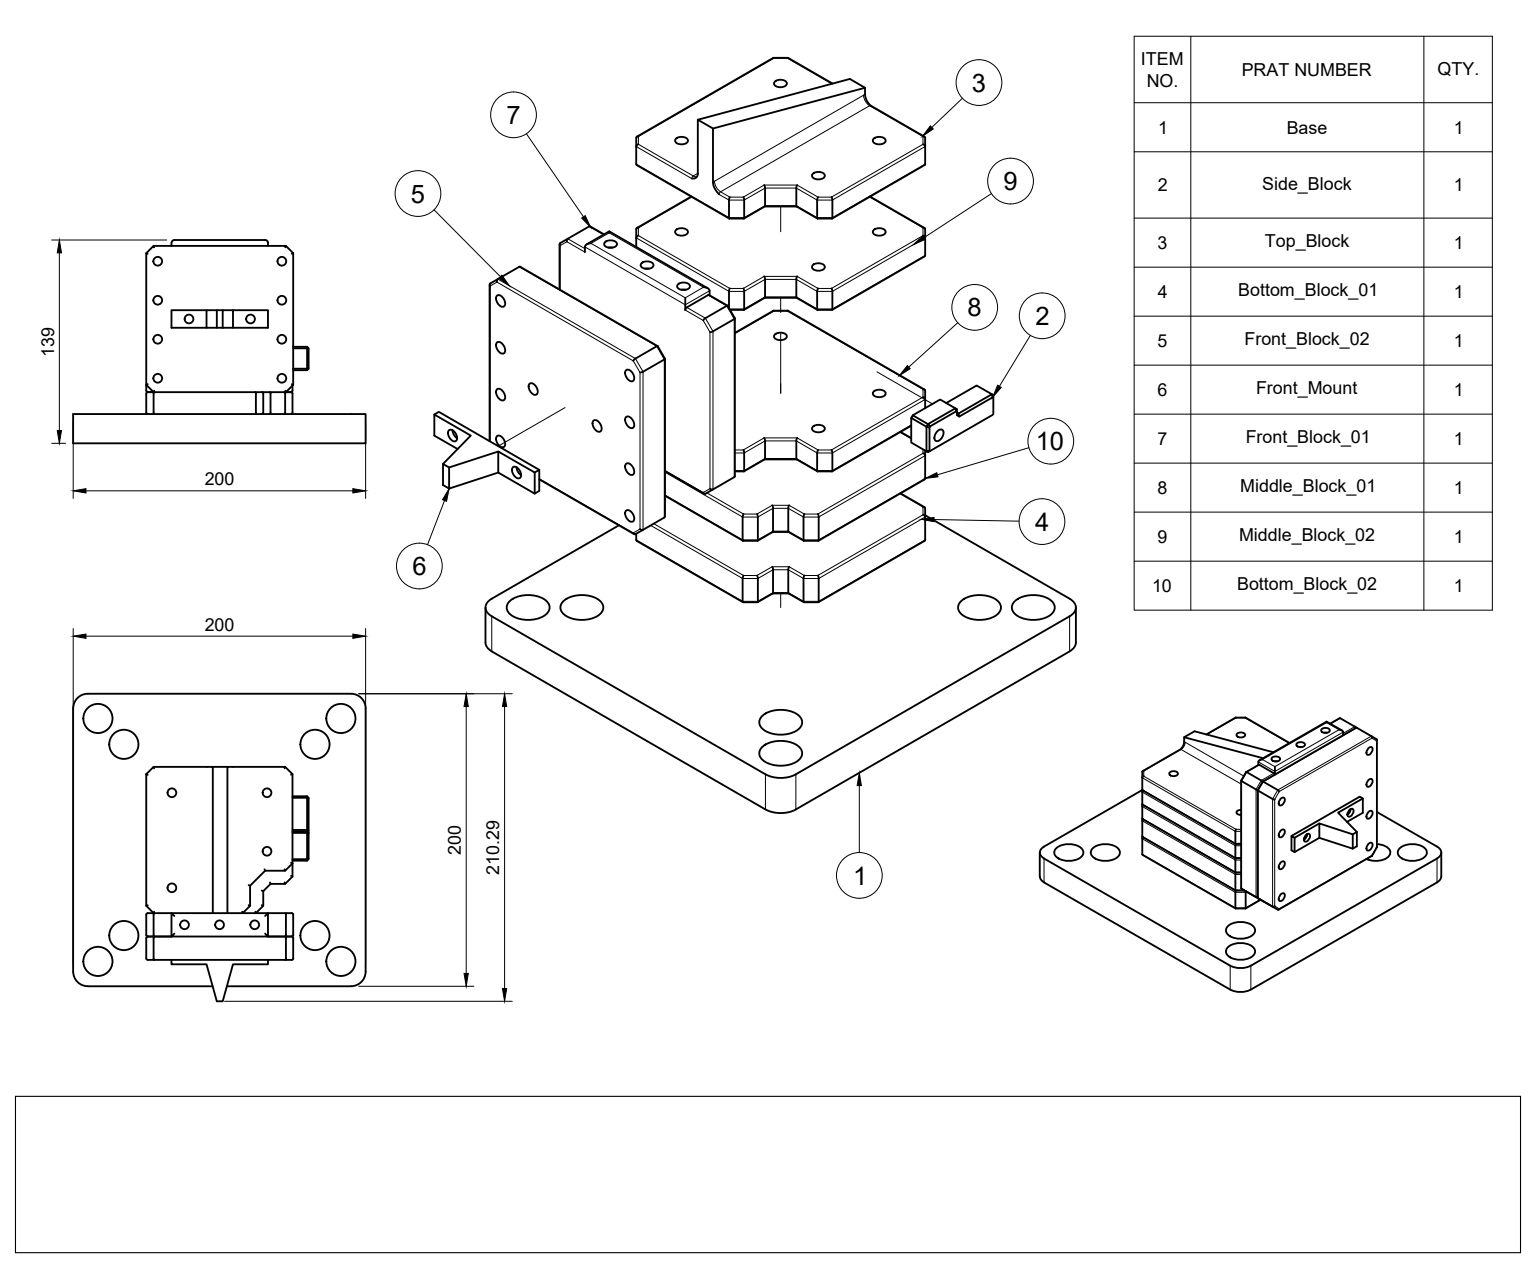
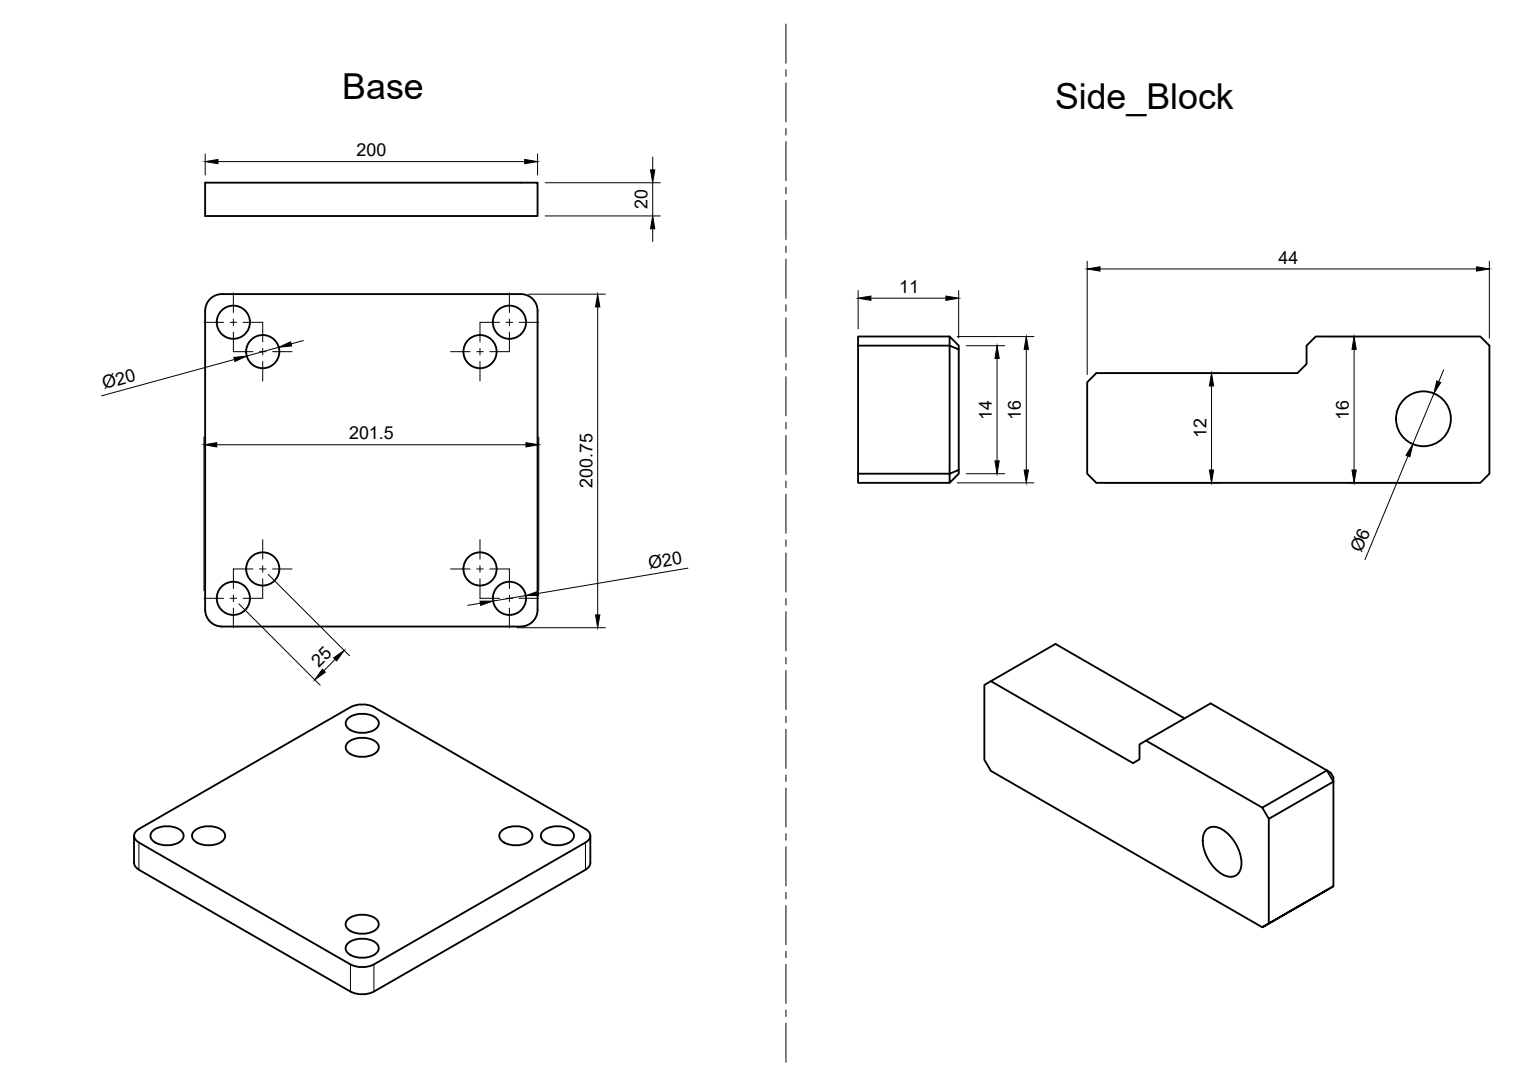
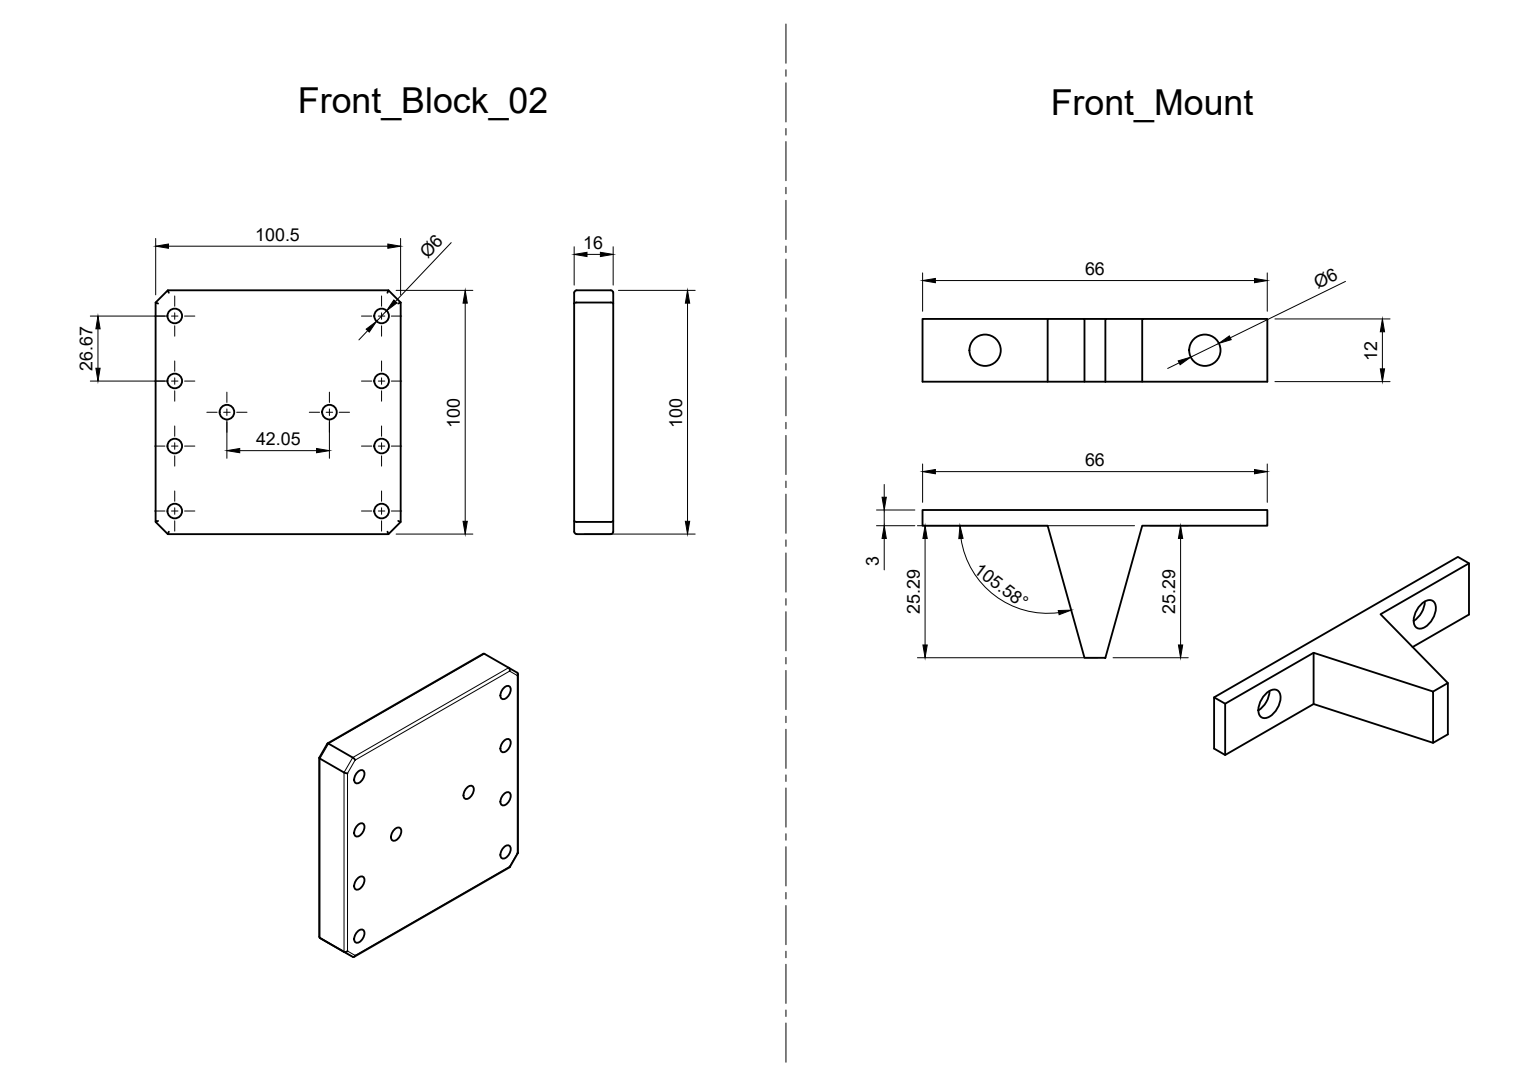
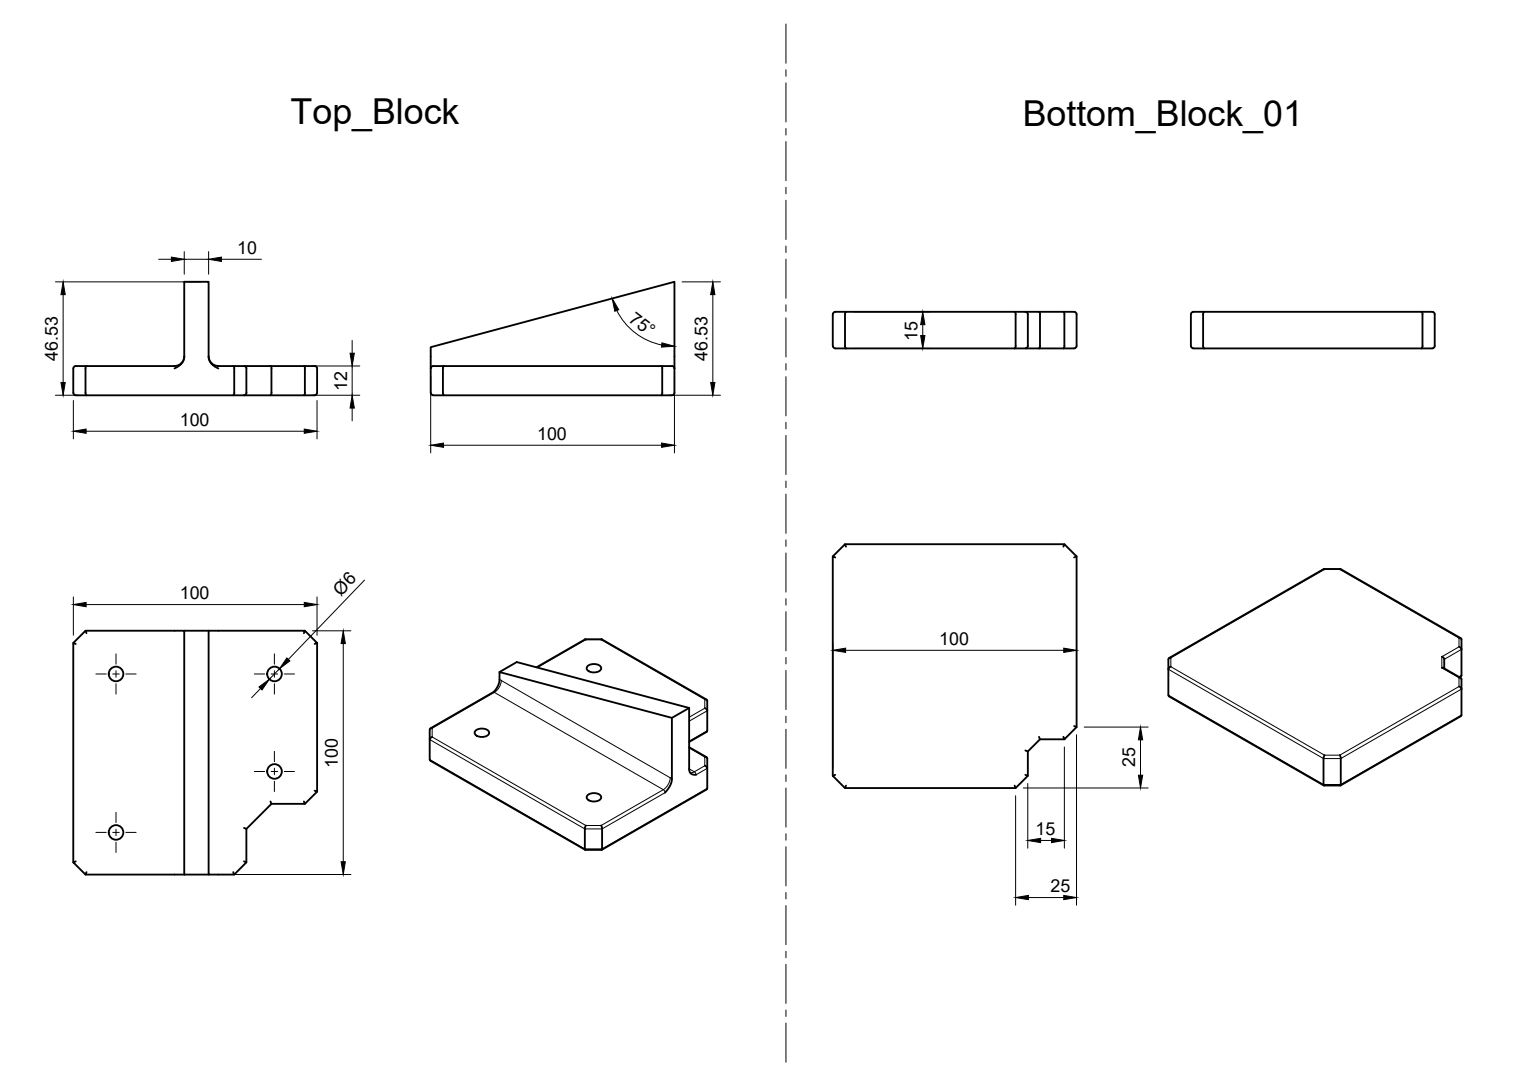
ISO-10303-21;
HEADER;
/* Generated by software containing ST-Developer
 * from STEP Tools, Inc. (www.steptools.com) 
 */

FILE_DESCRIPTION(
/* description */ (''),
/* implementation_level */ '2;1');

FILE_NAME(
/* name */ 'MAS-266',
/* time_stamp */ '2026-10-23T22:30:33+06:00',
/* author */ (''),
/* organization */ (''),
/* preprocessor_version */ 'ST-DEVELOPER v20.2',
/* originating_system */ 'Autodesk Translation Framework v15.15.0.0',
/* authorisation */ '');

FILE_SCHEMA (('AUTOMOTIVE_DESIGN { 1 0 10303 214 3 1 1 }'));
ENDSEC;

DATA;
#10=MECHANICAL_DESIGN_GEOMETRIC_PRESENTATION_REPRESENTATION('',(#235,#236,
#237,#238,#239,#240,#241,#242,#243,#244),#10131);
#11=ITEM_DEFINED_TRANSFORMATION($,$,#6001,#6612);
#12=ITEM_DEFINED_TRANSFORMATION($,$,#6044,#6613);
#13=ITEM_DEFINED_TRANSFORMATION($,$,#6074,#6614);
#14=ITEM_DEFINED_TRANSFORMATION($,$,#6173,#6615);
#15=ITEM_DEFINED_TRANSFORMATION($,$,#6236,#6616);
#16=ITEM_DEFINED_TRANSFORMATION($,$,#6309,#6617);
#17=ITEM_DEFINED_TRANSFORMATION($,$,#6326,#6618);
#18=ITEM_DEFINED_TRANSFORMATION($,$,#6399,#6619);
#19=ITEM_DEFINED_TRANSFORMATION($,$,#6474,#6620);
#20=ITEM_DEFINED_TRANSFORMATION($,$,#6549,#6621);
#21=(
REPRESENTATION_RELATIONSHIP($,$,#10169,#10168)
REPRESENTATION_RELATIONSHIP_WITH_TRANSFORMATION(#11)
SHAPE_REPRESENTATION_RELATIONSHIP()
);
#22=(
REPRESENTATION_RELATIONSHIP($,$,#10170,#10168)
REPRESENTATION_RELATIONSHIP_WITH_TRANSFORMATION(#12)
SHAPE_REPRESENTATION_RELATIONSHIP()
);
#23=(
REPRESENTATION_RELATIONSHIP($,$,#10171,#10168)
REPRESENTATION_RELATIONSHIP_WITH_TRANSFORMATION(#13)
SHAPE_REPRESENTATION_RELATIONSHIP()
);
#24=(
REPRESENTATION_RELATIONSHIP($,$,#10172,#10168)
REPRESENTATION_RELATIONSHIP_WITH_TRANSFORMATION(#14)
SHAPE_REPRESENTATION_RELATIONSHIP()
);
#25=(
REPRESENTATION_RELATIONSHIP($,$,#10173,#10168)
REPRESENTATION_RELATIONSHIP_WITH_TRANSFORMATION(#15)
SHAPE_REPRESENTATION_RELATIONSHIP()
);
#26=(
REPRESENTATION_RELATIONSHIP($,$,#10174,#10168)
REPRESENTATION_RELATIONSHIP_WITH_TRANSFORMATION(#16)
SHAPE_REPRESENTATION_RELATIONSHIP()
);
#27=(
REPRESENTATION_RELATIONSHIP($,$,#10175,#10168)
REPRESENTATION_RELATIONSHIP_WITH_TRANSFORMATION(#17)
SHAPE_REPRESENTATION_RELATIONSHIP()
);
#28=(
REPRESENTATION_RELATIONSHIP($,$,#10176,#10168)
REPRESENTATION_RELATIONSHIP_WITH_TRANSFORMATION(#18)
SHAPE_REPRESENTATION_RELATIONSHIP()
);
#29=(
REPRESENTATION_RELATIONSHIP($,$,#10177,#10168)
REPRESENTATION_RELATIONSHIP_WITH_TRANSFORMATION(#19)
SHAPE_REPRESENTATION_RELATIONSHIP()
);
#30=(
REPRESENTATION_RELATIONSHIP($,$,#10178,#10168)
REPRESENTATION_RELATIONSHIP_WITH_TRANSFORMATION(#20)
SHAPE_REPRESENTATION_RELATIONSHIP()
);
#31=CONTEXT_DEPENDENT_SHAPE_REPRESENTATION(#21,#10158);
#32=CONTEXT_DEPENDENT_SHAPE_REPRESENTATION(#22,#10159);
#33=CONTEXT_DEPENDENT_SHAPE_REPRESENTATION(#23,#10160);
#34=CONTEXT_DEPENDENT_SHAPE_REPRESENTATION(#24,#10161);
#35=CONTEXT_DEPENDENT_SHAPE_REPRESENTATION(#25,#10162);
#36=CONTEXT_DEPENDENT_SHAPE_REPRESENTATION(#26,#10163);
#37=CONTEXT_DEPENDENT_SHAPE_REPRESENTATION(#27,#10164);
#38=CONTEXT_DEPENDENT_SHAPE_REPRESENTATION(#28,#10165);
#39=CONTEXT_DEPENDENT_SHAPE_REPRESENTATION(#29,#10166);
#40=CONTEXT_DEPENDENT_SHAPE_REPRESENTATION(#30,#10167);
#41=NEXT_ASSEMBLY_USAGE_OCCURRENCE('Base:1','Base:1','Base:1',#10180,#10181,
'Base:1');
#42=NEXT_ASSEMBLY_USAGE_OCCURRENCE('Side_Block:1','Side_Block:1',
'Side_Block:1',#10180,#10182,'Side_Block:1');
#43=NEXT_ASSEMBLY_USAGE_OCCURRENCE('Top_Block:1','Top_Block:1',
'Top_Block:1',#10180,#10183,'Top_Block:1');
#44=NEXT_ASSEMBLY_USAGE_OCCURRENCE('Bottom_Block_01:1',
'Bottom_Block_01:1','Bottom_Block_01:1',#10180,#10184,
'Bottom_Block_01:1');
#45=NEXT_ASSEMBLY_USAGE_OCCURRENCE('Front_Block_02:1',
'Front_Block_02:1','Front_Block_02:1',#10180,#10185,'Front_Block_02:1');
#46=NEXT_ASSEMBLY_USAGE_OCCURRENCE('Front_Mount:1','Front_Mount:1',
'Front_Mount:1',#10180,#10186,'Front_Mount:1');
#47=NEXT_ASSEMBLY_USAGE_OCCURRENCE('Front_Block_01:1',
'Front_Block_01:1','Front_Block_01:1',#10180,#10187,'Front_Block_01:1');
#48=NEXT_ASSEMBLY_USAGE_OCCURRENCE('Middle_Block_01:1',
'Middle_Block_01:1','Middle_Block_01:1',#10180,#10188,
'Middle_Block_01:1');
#49=NEXT_ASSEMBLY_USAGE_OCCURRENCE('Middle_Block_02:1',
'Middle_Block_02:1','Middle_Block_02:1',#10180,#10189,
'Middle_Block_02:1');
#50=NEXT_ASSEMBLY_USAGE_OCCURRENCE('Bottom_Block_02:1',
'Bottom_Block_02:1','Bottom_Block_02:1',#10180,#10190,
'Bottom_Block_02:1');
#51=ELLIPSE('',#6109,1.08239220029239,1.);
#52=ELLIPSE('',#6111,1.08239220029239,1.);
#53=ELLIPSE('',#6115,1.08239220029239,1.);
#54=ELLIPSE('',#6117,1.08239220029239,1.);
#55=ELLIPSE('',#6119,1.0823922002924,1.);
#56=ELLIPSE('',#6120,1.08239220029239,1.);
#57=ELLIPSE('',#6122,1.08239220029239,1.);
#58=ELLIPSE('',#6123,1.0823922002924,1.);
#59=ELLIPSE('',#6125,1.0823922002924,1.);
#60=ELLIPSE('',#6127,1.0823922002924,1.);
#61=ELLIPSE('',#6128,1.0823922002924,1.);
#62=ELLIPSE('',#6130,1.08239220029239,1.);
#63=ELLIPSE('',#6133,1.08239220029239,1.);
#64=ELLIPSE('',#6135,1.0823922002924,1.);
#65=ELLIPSE('',#6138,1.08239220029239,1.);
#66=ELLIPSE('',#6140,1.0823922002924,1.);
#67=ELLIPSE('',#6150,1.08239220029239,1.);
#68=ELLIPSE('',#6152,1.08239220029239,1.);
#69=ELLIPSE('',#6155,1.08239220029239,1.);
#70=ELLIPSE('',#6157,1.0823922002924,1.);
#71=ELLIPSE('',#6159,1.08239220029239,1.);
#72=ELLIPSE('',#6161,1.08239220029239,1.);
#73=ELLIPSE('',#6163,1.0823922002924,1.);
#74=ELLIPSE('',#6165,1.0823922002924,1.);
#75=ELLIPSE('',#6175,1.08239220029239,1.);
#76=ELLIPSE('',#6176,1.08239220029239,1.);
#77=ELLIPSE('',#6178,1.08239220029239,1.);
#78=ELLIPSE('',#6179,1.08239220029239,1.);
#79=ELLIPSE('',#6181,1.08239220029239,1.);
#80=ELLIPSE('',#6183,1.0823922002924,1.);
#81=ELLIPSE('',#6185,1.08239220029239,1.);
#82=ELLIPSE('',#6187,1.0823922002924,1.);
#83=ELLIPSE('',#6189,1.08239220029239,1.);
#84=ELLIPSE('',#6191,1.0823922002924,1.);
#85=ELLIPSE('',#6193,1.08239220029239,1.);
#86=ELLIPSE('',#6195,1.0823922002924,1.);
#87=ELLIPSE('',#6206,1.08239220029239,1.);
#88=ELLIPSE('',#6207,1.0823922002924,1.);
#89=ELLIPSE('',#6209,1.08239220029239,1.);
#90=ELLIPSE('',#6211,1.0823922002924,1.);
#91=ELLIPSE('',#6213,1.08239220029239,1.);
#92=ELLIPSE('',#6215,1.0823922002924,1.);
#93=ELLIPSE('',#6217,1.08239220029239,1.);
#94=ELLIPSE('',#6219,1.0823922002924,1.);
#95=ELLIPSE('',#6221,1.08239220029239,1.);
#96=ELLIPSE('',#6223,1.0823922002924,1.);
#97=ELLIPSE('',#6225,1.08239220029239,1.);
#98=ELLIPSE('',#6227,1.08239220029239,1.);
#99=ELLIPSE('',#6268,1.0823922002924,1.);
#100=ELLIPSE('',#6269,1.0823922002924,1.);
#101=ELLIPSE('',#6271,1.08239220029239,1.);
#102=ELLIPSE('',#6273,1.0823922002924,1.);
#103=ELLIPSE('',#6275,1.08239220029239,1.);
#104=ELLIPSE('',#6277,1.0823922002924,1.);
#105=ELLIPSE('',#6279,1.0823922002924,1.);
#106=ELLIPSE('',#6281,1.08239220029239,1.);
#107=ELLIPSE('',#6289,1.0823922002924,1.);
#108=ELLIPSE('',#6290,1.08239220029239,1.);
#109=ELLIPSE('',#6292,1.08239220029239,1.);
#110=ELLIPSE('',#6294,1.08239220029239,1.);
#111=ELLIPSE('',#6296,1.08239220029239,1.);
#112=ELLIPSE('',#6298,1.0823922002924,1.);
#113=ELLIPSE('',#6300,1.08239220029239,1.);
#114=ELLIPSE('',#6302,1.0823922002924,1.);
#115=ELLIPSE('',#6340,2.82842712474619,2.);
#116=ELLIPSE('',#6341,2.82842712474619,2.);
#117=ELLIPSE('',#6343,2.8284271247462,2.);
#118=ELLIPSE('',#6345,2.8284271247462,2.);
#119=ELLIPSE('',#6357,1.08239220029239,1.);
#120=ELLIPSE('',#6359,1.0823922002924,1.);
#121=ELLIPSE('',#6362,1.0823922002924,1.);
#122=ELLIPSE('',#6364,1.0823922002924,1.);
#123=ELLIPSE('',#6365,1.0823922002924,1.);
#124=ELLIPSE('',#6367,1.08239220029239,1.);
#125=ELLIPSE('',#6369,1.0823922002924,1.);
#126=ELLIPSE('',#6371,1.08239220029239,1.);
#127=ELLIPSE('',#6373,1.0823922002924,1.);
#128=ELLIPSE('',#6381,1.0823922002924,1.);
#129=ELLIPSE('',#6382,1.08239220029239,1.);
#130=ELLIPSE('',#6384,1.08239220029239,1.);
#131=ELLIPSE('',#6386,1.08239220029239,1.);
#132=ELLIPSE('',#6388,1.08239220029239,1.);
#133=ELLIPSE('',#6390,1.0823922002924,1.);
#134=ELLIPSE('',#6392,1.08239220029239,1.);
#135=ELLIPSE('',#6413,1.0823922002924,1.);
#136=ELLIPSE('',#6414,1.08239220029239,1.);
#137=ELLIPSE('',#6416,1.08239220029239,1.);
#138=ELLIPSE('',#6417,1.0823922002924,1.);
#139=ELLIPSE('',#6419,1.0823922002924,1.);
#140=ELLIPSE('',#6421,1.0823922002924,1.);
#141=ELLIPSE('',#6422,1.0823922002924,1.);
#142=ELLIPSE('',#6424,1.08239220029239,1.);
#143=ELLIPSE('',#6427,1.08239220029239,1.);
#144=ELLIPSE('',#6429,1.0823922002924,1.);
#145=ELLIPSE('',#6432,1.08239220029239,1.);
#146=ELLIPSE('',#6434,1.0823922002924,1.);
#147=ELLIPSE('',#6444,1.08239220029239,1.);
#148=ELLIPSE('',#6445,1.08239220029239,1.);
#149=ELLIPSE('',#6447,1.08239220029239,1.);
#150=ELLIPSE('',#6449,1.08239220029239,1.);
#151=ELLIPSE('',#6451,1.08239220029239,1.);
#152=ELLIPSE('',#6453,1.08239220029239,1.);
#153=ELLIPSE('',#6455,1.0823922002924,1.);
#154=ELLIPSE('',#6457,1.08239220029239,1.);
#155=ELLIPSE('',#6459,1.08239220029239,1.);
#156=ELLIPSE('',#6461,1.0823922002924,1.);
#157=ELLIPSE('',#6463,1.0823922002924,1.);
#158=ELLIPSE('',#6465,1.08239220029239,1.);
#159=ELLIPSE('',#6488,1.0823922002924,1.);
#160=ELLIPSE('',#6489,1.08239220029239,1.);
#161=ELLIPSE('',#6491,1.08239220029239,1.);
#162=ELLIPSE('',#6492,1.0823922002924,1.);
#163=ELLIPSE('',#6494,1.0823922002924,1.);
#164=ELLIPSE('',#6496,1.0823922002924,1.);
#165=ELLIPSE('',#6497,1.0823922002924,1.);
#166=ELLIPSE('',#6499,1.08239220029239,1.);
#167=ELLIPSE('',#6502,1.08239220029239,1.);
#168=ELLIPSE('',#6504,1.0823922002924,1.);
#169=ELLIPSE('',#6507,1.08239220029239,1.);
#170=ELLIPSE('',#6509,1.0823922002924,1.);
#171=ELLIPSE('',#6519,1.08239220029239,1.);
#172=ELLIPSE('',#6520,1.08239220029239,1.);
#173=ELLIPSE('',#6522,1.08239220029239,1.);
#174=ELLIPSE('',#6524,1.08239220029239,1.);
#175=ELLIPSE('',#6526,1.08239220029239,1.);
#176=ELLIPSE('',#6528,1.08239220029239,1.);
#177=ELLIPSE('',#6530,1.0823922002924,1.);
#178=ELLIPSE('',#6532,1.08239220029239,1.);
#179=ELLIPSE('',#6534,1.08239220029239,1.);
#180=ELLIPSE('',#6536,1.0823922002924,1.);
#181=ELLIPSE('',#6538,1.0823922002924,1.);
#182=ELLIPSE('',#6540,1.08239220029239,1.);
#183=ELLIPSE('',#6551,1.08239220029239,1.);
#184=ELLIPSE('',#6552,1.08239220029239,1.);
#185=ELLIPSE('',#6554,1.08239220029239,1.);
#186=ELLIPSE('',#6555,1.08239220029239,1.);
#187=ELLIPSE('',#6557,1.08239220029239,1.);
#188=ELLIPSE('',#6559,1.0823922002924,1.);
#189=ELLIPSE('',#6561,1.08239220029239,1.);
#190=ELLIPSE('',#6563,1.0823922002924,1.);
#191=ELLIPSE('',#6565,1.08239220029239,1.);
#192=ELLIPSE('',#6567,1.0823922002924,1.);
#193=ELLIPSE('',#6569,1.08239220029239,1.);
#194=ELLIPSE('',#6571,1.0823922002924,1.);
#195=ELLIPSE('',#6582,1.08239220029239,1.);
#196=ELLIPSE('',#6583,1.0823922002924,1.);
#197=ELLIPSE('',#6585,1.08239220029239,1.);
#198=ELLIPSE('',#6587,1.0823922002924,1.);
#199=ELLIPSE('',#6589,1.08239220029239,1.);
#200=ELLIPSE('',#6591,1.0823922002924,1.);
#201=ELLIPSE('',#6593,1.08239220029239,1.);
#202=ELLIPSE('',#6595,1.0823922002924,1.);
#203=ELLIPSE('',#6597,1.08239220029239,1.);
#204=ELLIPSE('',#6599,1.0823922002924,1.);
#205=ELLIPSE('',#6601,1.08239220029239,1.);
#206=ELLIPSE('',#6603,1.08239220029239,1.);
#207=B_SPLINE_CURVE_WITH_KNOTS('',3,(#8653,#8654,#8655,#8656,#8657,#8658,
#8659,#8660,#8661,#8662),.UNSPECIFIED.,.F.,.F.,(4,2,2,2,4),(0.,0.179989683878213,
0.359979367756426,0.499959890996325,0.633875417351683),.UNSPECIFIED.);
#208=B_SPLINE_CURVE_WITH_KNOTS('',3,(#8673,#8674,#8675,#8676,#8677,#8678,
#8679,#8680,#8681,#8682),.UNSPECIFIED.,.F.,.F.,(4,2,2,2,4),(1.82590429893059,
1.95981982528595,2.09980034852585,2.27979003240406,2.45977971628227),
 .UNSPECIFIED.);
#209=B_SPLINE_CURVE_WITH_KNOTS('',3,(#8698,#8699,#8700,#8701,#8702,#8703,
#8704,#8705,#8706,#8707),.UNSPECIFIED.,.F.,.F.,(4,2,2,2,4),(0.,0.179989683878213,
0.359979367756426,0.499959890996325,0.633875417351683),.UNSPECIFIED.);
#210=B_SPLINE_CURVE_WITH_KNOTS('',3,(#8718,#8719,#8720,#8721,#8722,#8723,
#8724,#8725,#8726,#8727),.UNSPECIFIED.,.F.,.F.,(4,2,2,2,4),(1.82590429893059,
1.95981982528595,2.09980034852585,2.27979003240406,2.45977971628227),
 .UNSPECIFIED.);
#211=TOROIDAL_SURFACE('',#6075,5.,4.);
#212=TOROIDAL_SURFACE('',#6081,5.,4.);
#213=TOROIDAL_SURFACE('',#6085,5.,4.);
#214=TOROIDAL_SURFACE('',#6091,5.,4.);
#215=SHAPE_REPRESENTATION_RELATIONSHIP('SRR','None',#10169,#225);
#216=SHAPE_REPRESENTATION_RELATIONSHIP('SRR','None',#10170,#226);
#217=SHAPE_REPRESENTATION_RELATIONSHIP('SRR','None',#10171,#227);
#218=SHAPE_REPRESENTATION_RELATIONSHIP('SRR','None',#10172,#228);
#219=SHAPE_REPRESENTATION_RELATIONSHIP('SRR','None',#10173,#229);
#220=SHAPE_REPRESENTATION_RELATIONSHIP('SRR','None',#10174,#230);
#221=SHAPE_REPRESENTATION_RELATIONSHIP('SRR','None',#10175,#231);
#222=SHAPE_REPRESENTATION_RELATIONSHIP('SRR','None',#10176,#232);
#223=SHAPE_REPRESENTATION_RELATIONSHIP('SRR','None',#10177,#233);
#224=SHAPE_REPRESENTATION_RELATIONSHIP('SRR','None',#10178,#234);
#225=ADVANCED_BREP_SHAPE_REPRESENTATION('',(#245),#10121);
#226=ADVANCED_BREP_SHAPE_REPRESENTATION('',(#246),#10122);
#227=ADVANCED_BREP_SHAPE_REPRESENTATION('',(#247),#10123);
#228=ADVANCED_BREP_SHAPE_REPRESENTATION('',(#248),#10124);
#229=ADVANCED_BREP_SHAPE_REPRESENTATION('',(#249),#10125);
#230=ADVANCED_BREP_SHAPE_REPRESENTATION('',(#250),#10126);
#231=ADVANCED_BREP_SHAPE_REPRESENTATION('',(#251),#10127);
#232=ADVANCED_BREP_SHAPE_REPRESENTATION('',(#252),#10128);
#233=ADVANCED_BREP_SHAPE_REPRESENTATION('',(#253),#10129);
#234=ADVANCED_BREP_SHAPE_REPRESENTATION('',(#254),#10130);
#235=STYLED_ITEM('',(#10247),#245);
#236=STYLED_ITEM('',(#10247),#246);
#237=STYLED_ITEM('',(#10247),#247);
#238=STYLED_ITEM('',(#10247),#248);
#239=STYLED_ITEM('',(#10247),#249);
#240=STYLED_ITEM('',(#10261),#250);
#241=STYLED_ITEM('',(#10247),#251);
#242=STYLED_ITEM('',(#10247),#252);
#243=STYLED_ITEM('',(#10247),#253);
#244=STYLED_ITEM('',(#10247),#254);
#245=MANIFOLD_SOLID_BREP('Base',#5879);
#246=MANIFOLD_SOLID_BREP('Side_Block',#5880);
#247=MANIFOLD_SOLID_BREP('Top_Block',#5881);
#248=MANIFOLD_SOLID_BREP('Bottom_Block_01',#5882);
#249=MANIFOLD_SOLID_BREP('Front_Block_02',#5883);
#250=MANIFOLD_SOLID_BREP('Front_Mount',#5884);
#251=MANIFOLD_SOLID_BREP('Front_Block_01',#5885);
#252=MANIFOLD_SOLID_BREP('Middle_Block_01',#5886);
#253=MANIFOLD_SOLID_BREP('Middle_Block_02',#5887);
#254=MANIFOLD_SOLID_BREP('Bottom_Block_02',#5888);
#255=FACE_BOUND('',#827,.T.);
#256=FACE_BOUND('',#828,.T.);
#257=FACE_BOUND('',#829,.T.);
#258=FACE_BOUND('',#830,.T.);
#259=FACE_BOUND('',#831,.T.);
#260=FACE_BOUND('',#832,.T.);
#261=FACE_BOUND('',#833,.T.);
#262=FACE_BOUND('',#834,.T.);
#263=FACE_BOUND('',#842,.T.);
#264=FACE_BOUND('',#843,.T.);
#265=FACE_BOUND('',#844,.T.);
#266=FACE_BOUND('',#845,.T.);
#267=FACE_BOUND('',#846,.T.);
#268=FACE_BOUND('',#847,.T.);
#269=FACE_BOUND('',#848,.T.);
#270=FACE_BOUND('',#849,.T.);
#271=FACE_BOUND('',#870,.T.);
#272=FACE_BOUND('',#874,.T.);
#273=FACE_BOUND('',#895,.T.);
#274=FACE_BOUND('',#896,.T.);
#275=FACE_BOUND('',#898,.T.);
#276=FACE_BOUND('',#899,.T.);
#277=FACE_BOUND('',#921,.T.);
#278=FACE_BOUND('',#922,.T.);
#279=FACE_BOUND('',#923,.T.);
#280=FACE_BOUND('',#924,.T.);
#281=FACE_BOUND('',#1002,.T.);
#282=FACE_BOUND('',#1003,.T.);
#283=FACE_BOUND('',#1004,.T.);
#284=FACE_BOUND('',#1005,.T.);
#285=FACE_BOUND('',#1006,.T.);
#286=FACE_BOUND('',#1007,.T.);
#287=FACE_BOUND('',#1008,.T.);
#288=FACE_BOUND('',#1009,.T.);
#289=FACE_BOUND('',#1010,.T.);
#290=FACE_BOUND('',#1011,.T.);
#291=FACE_BOUND('',#1024,.T.);
#292=FACE_BOUND('',#1025,.T.);
#293=FACE_BOUND('',#1026,.T.);
#294=FACE_BOUND('',#1027,.T.);
#295=FACE_BOUND('',#1028,.T.);
#296=FACE_BOUND('',#1029,.T.);
#297=FACE_BOUND('',#1030,.T.);
#298=FACE_BOUND('',#1031,.T.);
#299=FACE_BOUND('',#1032,.T.);
#300=FACE_BOUND('',#1033,.T.);
#301=FACE_BOUND('',#1040,.T.);
#302=FACE_BOUND('',#1043,.T.);
#303=FACE_BOUND('',#1044,.T.);
#304=FACE_BOUND('',#1047,.T.);
#305=FACE_BOUND('',#1064,.T.);
#306=FACE_BOUND('',#1065,.T.);
#307=FACE_BOUND('',#1066,.T.);
#308=FACE_BOUND('',#1119,.T.);
#309=FACE_BOUND('',#1120,.T.);
#310=FACE_BOUND('',#1121,.T.);
#311=FACE_BOUND('',#1122,.T.);
#312=FACE_BOUND('',#1138,.T.);
#313=FACE_BOUND('',#1139,.T.);
#314=FACE_BOUND('',#1140,.T.);
#315=FACE_BOUND('',#1141,.T.);
#316=FACE_BOUND('',#1169,.T.);
#317=FACE_BOUND('',#1170,.T.);
#318=FACE_BOUND('',#1171,.T.);
#319=FACE_BOUND('',#1172,.T.);
#320=FACE_BOUND('',#1188,.T.);
#321=FACE_BOUND('',#1189,.T.);
#322=FACE_BOUND('',#1190,.T.);
#323=FACE_BOUND('',#1191,.T.);
#324=PLANE('',#6029);
#325=PLANE('',#6030);
#326=PLANE('',#6036);
#327=PLANE('',#6041);
#328=PLANE('',#6042);
#329=PLANE('',#6043);
#330=PLANE('',#6048);
#331=PLANE('',#6049);
#332=PLANE('',#6050);
#333=PLANE('',#6051);
#334=PLANE('',#6052);
#335=PLANE('',#6053);
#336=PLANE('',#6054);
#337=PLANE('',#6055);
#338=PLANE('',#6056);
#339=PLANE('',#6057);
#340=PLANE('',#6058);
#341=PLANE('',#6059);
#342=PLANE('',#6060);
#343=PLANE('',#6061);
#344=PLANE('',#6062);
#345=PLANE('',#6063);
#346=PLANE('',#6064);
#347=PLANE('',#6065);
#348=PLANE('',#6066);
#349=PLANE('',#6067);
#350=PLANE('',#6068);
#351=PLANE('',#6069);
#352=PLANE('',#6070);
#353=PLANE('',#6071);
#354=PLANE('',#6072);
#355=PLANE('',#6073);
#356=PLANE('',#6084);
#357=PLANE('',#6094);
#358=PLANE('',#6107);
#359=PLANE('',#6112);
#360=PLANE('',#6113);
#361=PLANE('',#6142);
#362=PLANE('',#6143);
#363=PLANE('',#6144);
#364=PLANE('',#6145);
#365=PLANE('',#6146);
#366=PLANE('',#6147);
#367=PLANE('',#6148);
#368=PLANE('',#6167);
#369=PLANE('',#6168);
#370=PLANE('',#6169);
#371=PLANE('',#6170);
#372=PLANE('',#6171);
#373=PLANE('',#6172);
#374=PLANE('',#6198);
#375=PLANE('',#6199);
#376=PLANE('',#6200);
#377=PLANE('',#6201);
#378=PLANE('',#6202);
#379=PLANE('',#6203);
#380=PLANE('',#6204);
#381=PLANE('',#6229);
#382=PLANE('',#6230);
#383=PLANE('',#6231);
#384=PLANE('',#6232);
#385=PLANE('',#6233);
#386=PLANE('',#6234);
#387=PLANE('',#6235);
#388=PLANE('',#6283);
#389=PLANE('',#6284);
#390=PLANE('',#6285);
#391=PLANE('',#6286);
#392=PLANE('',#6287);
#393=PLANE('',#6304);
#394=PLANE('',#6305);
#395=PLANE('',#6306);
#396=PLANE('',#6307);
#397=PLANE('',#6308);
#398=PLANE('',#6316);
#399=PLANE('',#6317);
#400=PLANE('',#6318);
#401=PLANE('',#6319);
#402=PLANE('',#6320);
#403=PLANE('',#6321);
#404=PLANE('',#6322);
#405=PLANE('',#6323);
#406=PLANE('',#6324);
#407=PLANE('',#6325);
#408=PLANE('',#6330);
#409=PLANE('',#6334);
#410=PLANE('',#6338);
#411=PLANE('',#6347);
#412=PLANE('',#6350);
#413=PLANE('',#6351);
#414=PLANE('',#6352);
#415=PLANE('',#6355);
#416=PLANE('',#6360);
#417=PLANE('',#6376);
#418=PLANE('',#6377);
#419=PLANE('',#6378);
#420=PLANE('',#6379);
#421=PLANE('',#6395);
#422=PLANE('',#6396);
#423=PLANE('',#6397);
#424=PLANE('',#6398);
#425=PLANE('',#6436);
#426=PLANE('',#6437);
#427=PLANE('',#6438);
#428=PLANE('',#6439);
#429=PLANE('',#6440);
#430=PLANE('',#6441);
#431=PLANE('',#6442);
#432=PLANE('',#6467);
#433=PLANE('',#6468);
#434=PLANE('',#6469);
#435=PLANE('',#6470);
#436=PLANE('',#6471);
#437=PLANE('',#6472);
#438=PLANE('',#6473);
#439=PLANE('',#6511);
#440=PLANE('',#6512);
#441=PLANE('',#6513);
#442=PLANE('',#6514);
#443=PLANE('',#6515);
#444=PLANE('',#6516);
#445=PLANE('',#6517);
#446=PLANE('',#6542);
#447=PLANE('',#6543);
#448=PLANE('',#6544);
#449=PLANE('',#6545);
#450=PLANE('',#6546);
#451=PLANE('',#6547);
#452=PLANE('',#6548);
#453=PLANE('',#6574);
#454=PLANE('',#6575);
#455=PLANE('',#6576);
#456=PLANE('',#6577);
#457=PLANE('',#6578);
#458=PLANE('',#6579);
#459=PLANE('',#6580);
#460=PLANE('',#6605);
#461=PLANE('',#6606);
#462=PLANE('',#6607);
#463=PLANE('',#6608);
#464=PLANE('',#6609);
#465=PLANE('',#6610);
#466=PLANE('',#6611);
#467=FACE_OUTER_BOUND('',#816,.T.);
#468=FACE_OUTER_BOUND('',#817,.T.);
#469=FACE_OUTER_BOUND('',#818,.T.);
#470=FACE_OUTER_BOUND('',#819,.T.);
#471=FACE_OUTER_BOUND('',#820,.T.);
#472=FACE_OUTER_BOUND('',#821,.T.);
#473=FACE_OUTER_BOUND('',#822,.T.);
#474=FACE_OUTER_BOUND('',#823,.T.);
#475=FACE_OUTER_BOUND('',#824,.T.);
#476=FACE_OUTER_BOUND('',#825,.T.);
#477=FACE_OUTER_BOUND('',#826,.T.);
#478=FACE_OUTER_BOUND('',#835,.T.);
#479=FACE_OUTER_BOUND('',#836,.T.);
#480=FACE_OUTER_BOUND('',#837,.T.);
#481=FACE_OUTER_BOUND('',#838,.T.);
#482=FACE_OUTER_BOUND('',#839,.T.);
#483=FACE_OUTER_BOUND('',#840,.T.);
#484=FACE_OUTER_BOUND('',#841,.T.);
#485=FACE_OUTER_BOUND('',#850,.T.);
#486=FACE_OUTER_BOUND('',#851,.T.);
#487=FACE_OUTER_BOUND('',#852,.T.);
#488=FACE_OUTER_BOUND('',#853,.T.);
#489=FACE_OUTER_BOUND('',#854,.T.);
#490=FACE_OUTER_BOUND('',#855,.T.);
#491=FACE_OUTER_BOUND('',#856,.T.);
#492=FACE_OUTER_BOUND('',#857,.T.);
#493=FACE_OUTER_BOUND('',#858,.T.);
#494=FACE_OUTER_BOUND('',#859,.T.);
#495=FACE_OUTER_BOUND('',#860,.T.);
#496=FACE_OUTER_BOUND('',#861,.T.);
#497=FACE_OUTER_BOUND('',#862,.T.);
#498=FACE_OUTER_BOUND('',#863,.T.);
#499=FACE_OUTER_BOUND('',#864,.T.);
#500=FACE_OUTER_BOUND('',#865,.T.);
#501=FACE_OUTER_BOUND('',#866,.T.);
#502=FACE_OUTER_BOUND('',#867,.T.);
#503=FACE_OUTER_BOUND('',#868,.T.);
#504=FACE_OUTER_BOUND('',#869,.T.);
#505=FACE_OUTER_BOUND('',#871,.T.);
#506=FACE_OUTER_BOUND('',#872,.T.);
#507=FACE_OUTER_BOUND('',#873,.T.);
#508=FACE_OUTER_BOUND('',#875,.T.);
#509=FACE_OUTER_BOUND('',#876,.T.);
#510=FACE_OUTER_BOUND('',#877,.T.);
#511=FACE_OUTER_BOUND('',#878,.T.);
#512=FACE_OUTER_BOUND('',#879,.T.);
#513=FACE_OUTER_BOUND('',#880,.T.);
#514=FACE_OUTER_BOUND('',#881,.T.);
#515=FACE_OUTER_BOUND('',#882,.T.);
#516=FACE_OUTER_BOUND('',#883,.T.);
#517=FACE_OUTER_BOUND('',#884,.T.);
#518=FACE_OUTER_BOUND('',#885,.T.);
#519=FACE_OUTER_BOUND('',#886,.T.);
#520=FACE_OUTER_BOUND('',#887,.T.);
#521=FACE_OUTER_BOUND('',#888,.T.);
#522=FACE_OUTER_BOUND('',#889,.T.);
#523=FACE_OUTER_BOUND('',#890,.T.);
#524=FACE_OUTER_BOUND('',#891,.T.);
#525=FACE_OUTER_BOUND('',#892,.T.);
#526=FACE_OUTER_BOUND('',#893,.T.);
#527=FACE_OUTER_BOUND('',#894,.T.);
#528=FACE_OUTER_BOUND('',#897,.T.);
#529=FACE_OUTER_BOUND('',#900,.T.);
#530=FACE_OUTER_BOUND('',#901,.T.);
#531=FACE_OUTER_BOUND('',#902,.T.);
#532=FACE_OUTER_BOUND('',#903,.T.);
#533=FACE_OUTER_BOUND('',#904,.T.);
#534=FACE_OUTER_BOUND('',#905,.T.);
#535=FACE_OUTER_BOUND('',#906,.T.);
#536=FACE_OUTER_BOUND('',#907,.T.);
#537=FACE_OUTER_BOUND('',#908,.T.);
#538=FACE_OUTER_BOUND('',#909,.T.);
#539=FACE_OUTER_BOUND('',#910,.T.);
#540=FACE_OUTER_BOUND('',#911,.T.);
#541=FACE_OUTER_BOUND('',#912,.T.);
#542=FACE_OUTER_BOUND('',#913,.T.);
#543=FACE_OUTER_BOUND('',#914,.T.);
#544=FACE_OUTER_BOUND('',#915,.T.);
#545=FACE_OUTER_BOUND('',#916,.T.);
#546=FACE_OUTER_BOUND('',#917,.T.);
#547=FACE_OUTER_BOUND('',#918,.T.);
#548=FACE_OUTER_BOUND('',#919,.T.);
#549=FACE_OUTER_BOUND('',#920,.T.);
#550=FACE_OUTER_BOUND('',#925,.T.);
#551=FACE_OUTER_BOUND('',#926,.T.);
#552=FACE_OUTER_BOUND('',#927,.T.);
#553=FACE_OUTER_BOUND('',#928,.T.);
#554=FACE_OUTER_BOUND('',#929,.T.);
#555=FACE_OUTER_BOUND('',#930,.T.);
#556=FACE_OUTER_BOUND('',#931,.T.);
#557=FACE_OUTER_BOUND('',#932,.T.);
#558=FACE_OUTER_BOUND('',#933,.T.);
#559=FACE_OUTER_BOUND('',#934,.T.);
#560=FACE_OUTER_BOUND('',#935,.T.);
#561=FACE_OUTER_BOUND('',#936,.T.);
#562=FACE_OUTER_BOUND('',#937,.T.);
#563=FACE_OUTER_BOUND('',#938,.T.);
#564=FACE_OUTER_BOUND('',#939,.T.);
#565=FACE_OUTER_BOUND('',#940,.T.);
#566=FACE_OUTER_BOUND('',#941,.T.);
#567=FACE_OUTER_BOUND('',#942,.T.);
#568=FACE_OUTER_BOUND('',#943,.T.);
#569=FACE_OUTER_BOUND('',#944,.T.);
#570=FACE_OUTER_BOUND('',#945,.T.);
#571=FACE_OUTER_BOUND('',#946,.T.);
#572=FACE_OUTER_BOUND('',#947,.T.);
#573=FACE_OUTER_BOUND('',#948,.T.);
#574=FACE_OUTER_BOUND('',#949,.T.);
#575=FACE_OUTER_BOUND('',#950,.T.);
#576=FACE_OUTER_BOUND('',#951,.T.);
#577=FACE_OUTER_BOUND('',#952,.T.);
#578=FACE_OUTER_BOUND('',#953,.T.);
#579=FACE_OUTER_BOUND('',#954,.T.);
#580=FACE_OUTER_BOUND('',#955,.T.);
#581=FACE_OUTER_BOUND('',#956,.T.);
#582=FACE_OUTER_BOUND('',#957,.T.);
#583=FACE_OUTER_BOUND('',#958,.T.);
#584=FACE_OUTER_BOUND('',#959,.T.);
#585=FACE_OUTER_BOUND('',#960,.T.);
#586=FACE_OUTER_BOUND('',#961,.T.);
#587=FACE_OUTER_BOUND('',#962,.T.);
#588=FACE_OUTER_BOUND('',#963,.T.);
#589=FACE_OUTER_BOUND('',#964,.T.);
#590=FACE_OUTER_BOUND('',#965,.T.);
#591=FACE_OUTER_BOUND('',#966,.T.);
#592=FACE_OUTER_BOUND('',#967,.T.);
#593=FACE_OUTER_BOUND('',#968,.T.);
#594=FACE_OUTER_BOUND('',#969,.T.);
#595=FACE_OUTER_BOUND('',#970,.T.);
#596=FACE_OUTER_BOUND('',#971,.T.);
#597=FACE_OUTER_BOUND('',#972,.T.);
#598=FACE_OUTER_BOUND('',#973,.T.);
#599=FACE_OUTER_BOUND('',#974,.T.);
#600=FACE_OUTER_BOUND('',#975,.T.);
#601=FACE_OUTER_BOUND('',#976,.T.);
#602=FACE_OUTER_BOUND('',#977,.T.);
#603=FACE_OUTER_BOUND('',#978,.T.);
#604=FACE_OUTER_BOUND('',#979,.T.);
#605=FACE_OUTER_BOUND('',#980,.T.);
#606=FACE_OUTER_BOUND('',#981,.T.);
#607=FACE_OUTER_BOUND('',#982,.T.);
#608=FACE_OUTER_BOUND('',#983,.T.);
#609=FACE_OUTER_BOUND('',#984,.T.);
#610=FACE_OUTER_BOUND('',#985,.T.);
#611=FACE_OUTER_BOUND('',#986,.T.);
#612=FACE_OUTER_BOUND('',#987,.T.);
#613=FACE_OUTER_BOUND('',#988,.T.);
#614=FACE_OUTER_BOUND('',#989,.T.);
#615=FACE_OUTER_BOUND('',#990,.T.);
#616=FACE_OUTER_BOUND('',#991,.T.);
#617=FACE_OUTER_BOUND('',#992,.T.);
#618=FACE_OUTER_BOUND('',#993,.T.);
#619=FACE_OUTER_BOUND('',#994,.T.);
#620=FACE_OUTER_BOUND('',#995,.T.);
#621=FACE_OUTER_BOUND('',#996,.T.);
#622=FACE_OUTER_BOUND('',#997,.T.);
#623=FACE_OUTER_BOUND('',#998,.T.);
#624=FACE_OUTER_BOUND('',#999,.T.);
#625=FACE_OUTER_BOUND('',#1000,.T.);
#626=FACE_OUTER_BOUND('',#1001,.T.);
#627=FACE_OUTER_BOUND('',#1012,.T.);
#628=FACE_OUTER_BOUND('',#1013,.T.);
#629=FACE_OUTER_BOUND('',#1014,.T.);
#630=FACE_OUTER_BOUND('',#1015,.T.);
#631=FACE_OUTER_BOUND('',#1016,.T.);
#632=FACE_OUTER_BOUND('',#1017,.T.);
#633=FACE_OUTER_BOUND('',#1018,.T.);
#634=FACE_OUTER_BOUND('',#1019,.T.);
#635=FACE_OUTER_BOUND('',#1020,.T.);
#636=FACE_OUTER_BOUND('',#1021,.T.);
#637=FACE_OUTER_BOUND('',#1022,.T.);
#638=FACE_OUTER_BOUND('',#1023,.T.);
#639=FACE_OUTER_BOUND('',#1034,.T.);
#640=FACE_OUTER_BOUND('',#1035,.T.);
#641=FACE_OUTER_BOUND('',#1036,.T.);
#642=FACE_OUTER_BOUND('',#1037,.T.);
#643=FACE_OUTER_BOUND('',#1038,.T.);
#644=FACE_OUTER_BOUND('',#1039,.T.);
#645=FACE_OUTER_BOUND('',#1041,.T.);
#646=FACE_OUTER_BOUND('',#1042,.T.);
#647=FACE_OUTER_BOUND('',#1045,.T.);
#648=FACE_OUTER_BOUND('',#1046,.T.);
#649=FACE_OUTER_BOUND('',#1048,.T.);
#650=FACE_OUTER_BOUND('',#1049,.T.);
#651=FACE_OUTER_BOUND('',#1050,.T.);
#652=FACE_OUTER_BOUND('',#1051,.T.);
#653=FACE_OUTER_BOUND('',#1052,.T.);
#654=FACE_OUTER_BOUND('',#1053,.T.);
#655=FACE_OUTER_BOUND('',#1054,.T.);
#656=FACE_OUTER_BOUND('',#1055,.T.);
#657=FACE_OUTER_BOUND('',#1056,.T.);
#658=FACE_OUTER_BOUND('',#1057,.T.);
#659=FACE_OUTER_BOUND('',#1058,.T.);
#660=FACE_OUTER_BOUND('',#1059,.T.);
#661=FACE_OUTER_BOUND('',#1060,.T.);
#662=FACE_OUTER_BOUND('',#1061,.T.);
#663=FACE_OUTER_BOUND('',#1062,.T.);
#664=FACE_OUTER_BOUND('',#1063,.T.);
#665=FACE_OUTER_BOUND('',#1067,.T.);
#666=FACE_OUTER_BOUND('',#1068,.T.);
#667=FACE_OUTER_BOUND('',#1069,.T.);
#668=FACE_OUTER_BOUND('',#1070,.T.);
#669=FACE_OUTER_BOUND('',#1071,.T.);
#670=FACE_OUTER_BOUND('',#1072,.T.);
#671=FACE_OUTER_BOUND('',#1073,.T.);
#672=FACE_OUTER_BOUND('',#1074,.T.);
#673=FACE_OUTER_BOUND('',#1075,.T.);
#674=FACE_OUTER_BOUND('',#1076,.T.);
#675=FACE_OUTER_BOUND('',#1077,.T.);
#676=FACE_OUTER_BOUND('',#1078,.T.);
#677=FACE_OUTER_BOUND('',#1079,.T.);
#678=FACE_OUTER_BOUND('',#1080,.T.);
#679=FACE_OUTER_BOUND('',#1081,.T.);
#680=FACE_OUTER_BOUND('',#1082,.T.);
#681=FACE_OUTER_BOUND('',#1083,.T.);
#682=FACE_OUTER_BOUND('',#1084,.T.);
#683=FACE_OUTER_BOUND('',#1085,.T.);
#684=FACE_OUTER_BOUND('',#1086,.T.);
#685=FACE_OUTER_BOUND('',#1087,.T.);
#686=FACE_OUTER_BOUND('',#1088,.T.);
#687=FACE_OUTER_BOUND('',#1089,.T.);
#688=FACE_OUTER_BOUND('',#1090,.T.);
#689=FACE_OUTER_BOUND('',#1091,.T.);
#690=FACE_OUTER_BOUND('',#1092,.T.);
#691=FACE_OUTER_BOUND('',#1093,.T.);
#692=FACE_OUTER_BOUND('',#1094,.T.);
#693=FACE_OUTER_BOUND('',#1095,.T.);
#694=FACE_OUTER_BOUND('',#1096,.T.);
#695=FACE_OUTER_BOUND('',#1097,.T.);
#696=FACE_OUTER_BOUND('',#1098,.T.);
#697=FACE_OUTER_BOUND('',#1099,.T.);
#698=FACE_OUTER_BOUND('',#1100,.T.);
#699=FACE_OUTER_BOUND('',#1101,.T.);
#700=FACE_OUTER_BOUND('',#1102,.T.);
#701=FACE_OUTER_BOUND('',#1103,.T.);
#702=FACE_OUTER_BOUND('',#1104,.T.);
#703=FACE_OUTER_BOUND('',#1105,.T.);
#704=FACE_OUTER_BOUND('',#1106,.T.);
#705=FACE_OUTER_BOUND('',#1107,.T.);
#706=FACE_OUTER_BOUND('',#1108,.T.);
#707=FACE_OUTER_BOUND('',#1109,.T.);
#708=FACE_OUTER_BOUND('',#1110,.T.);
#709=FACE_OUTER_BOUND('',#1111,.T.);
#710=FACE_OUTER_BOUND('',#1112,.T.);
#711=FACE_OUTER_BOUND('',#1113,.T.);
#712=FACE_OUTER_BOUND('',#1114,.T.);
#713=FACE_OUTER_BOUND('',#1115,.T.);
#714=FACE_OUTER_BOUND('',#1116,.T.);
#715=FACE_OUTER_BOUND('',#1117,.T.);
#716=FACE_OUTER_BOUND('',#1118,.T.);
#717=FACE_OUTER_BOUND('',#1123,.T.);
#718=FACE_OUTER_BOUND('',#1124,.T.);
#719=FACE_OUTER_BOUND('',#1125,.T.);
#720=FACE_OUTER_BOUND('',#1126,.T.);
#721=FACE_OUTER_BOUND('',#1127,.T.);
#722=FACE_OUTER_BOUND('',#1128,.T.);
#723=FACE_OUTER_BOUND('',#1129,.T.);
#724=FACE_OUTER_BOUND('',#1130,.T.);
#725=FACE_OUTER_BOUND('',#1131,.T.);
#726=FACE_OUTER_BOUND('',#1132,.T.);
#727=FACE_OUTER_BOUND('',#1133,.T.);
#728=FACE_OUTER_BOUND('',#1134,.T.);
#729=FACE_OUTER_BOUND('',#1135,.T.);
#730=FACE_OUTER_BOUND('',#1136,.T.);
#731=FACE_OUTER_BOUND('',#1137,.T.);
#732=FACE_OUTER_BOUND('',#1142,.T.);
#733=FACE_OUTER_BOUND('',#1143,.T.);
#734=FACE_OUTER_BOUND('',#1144,.T.);
#735=FACE_OUTER_BOUND('',#1145,.T.);
#736=FACE_OUTER_BOUND('',#1146,.T.);
#737=FACE_OUTER_BOUND('',#1147,.T.);
#738=FACE_OUTER_BOUND('',#1148,.T.);
#739=FACE_OUTER_BOUND('',#1149,.T.);
#740=FACE_OUTER_BOUND('',#1150,.T.);
#741=FACE_OUTER_BOUND('',#1151,.T.);
#742=FACE_OUTER_BOUND('',#1152,.T.);
#743=FACE_OUTER_BOUND('',#1153,.T.);
#744=FACE_OUTER_BOUND('',#1154,.T.);
#745=FACE_OUTER_BOUND('',#1155,.T.);
#746=FACE_OUTER_BOUND('',#1156,.T.);
#747=FACE_OUTER_BOUND('',#1157,.T.);
#748=FACE_OUTER_BOUND('',#1158,.T.);
#749=FACE_OUTER_BOUND('',#1159,.T.);
#750=FACE_OUTER_BOUND('',#1160,.T.);
#751=FACE_OUTER_BOUND('',#1161,.T.);
#752=FACE_OUTER_BOUND('',#1162,.T.);
#753=FACE_OUTER_BOUND('',#1163,.T.);
#754=FACE_OUTER_BOUND('',#1164,.T.);
#755=FACE_OUTER_BOUND('',#1165,.T.);
#756=FACE_OUTER_BOUND('',#1166,.T.);
#757=FACE_OUTER_BOUND('',#1167,.T.);
#758=FACE_OUTER_BOUND('',#1168,.T.);
#759=FACE_OUTER_BOUND('',#1173,.T.);
#760=FACE_OUTER_BOUND('',#1174,.T.);
#761=FACE_OUTER_BOUND('',#1175,.T.);
#762=FACE_OUTER_BOUND('',#1176,.T.);
#763=FACE_OUTER_BOUND('',#1177,.T.);
#764=FACE_OUTER_BOUND('',#1178,.T.);
#765=FACE_OUTER_BOUND('',#1179,.T.);
#766=FACE_OUTER_BOUND('',#1180,.T.);
#767=FACE_OUTER_BOUND('',#1181,.T.);
#768=FACE_OUTER_BOUND('',#1182,.T.);
#769=FACE_OUTER_BOUND('',#1183,.T.);
#770=FACE_OUTER_BOUND('',#1184,.T.);
#771=FACE_OUTER_BOUND('',#1185,.T.);
#772=FACE_OUTER_BOUND('',#1186,.T.);
#773=FACE_OUTER_BOUND('',#1187,.T.);
#774=FACE_OUTER_BOUND('',#1192,.T.);
#775=FACE_OUTER_BOUND('',#1193,.T.);
#776=FACE_OUTER_BOUND('',#1194,.T.);
#777=FACE_OUTER_BOUND('',#1195,.T.);
#778=FACE_OUTER_BOUND('',#1196,.T.);
#779=FACE_OUTER_BOUND('',#1197,.T.);
#780=FACE_OUTER_BOUND('',#1198,.T.);
#781=FACE_OUTER_BOUND('',#1199,.T.);
#782=FACE_OUTER_BOUND('',#1200,.T.);
#783=FACE_OUTER_BOUND('',#1201,.T.);
#784=FACE_OUTER_BOUND('',#1202,.T.);
#785=FACE_OUTER_BOUND('',#1203,.T.);
#786=FACE_OUTER_BOUND('',#1204,.T.);
#787=FACE_OUTER_BOUND('',#1205,.T.);
#788=FACE_OUTER_BOUND('',#1206,.T.);
#789=FACE_OUTER_BOUND('',#1207,.T.);
#790=FACE_OUTER_BOUND('',#1208,.T.);
#791=FACE_OUTER_BOUND('',#1209,.T.);
#792=FACE_OUTER_BOUND('',#1210,.T.);
#793=FACE_OUTER_BOUND('',#1211,.T.);
#794=FACE_OUTER_BOUND('',#1212,.T.);
#795=FACE_OUTER_BOUND('',#1213,.T.);
#796=FACE_OUTER_BOUND('',#1214,.T.);
#797=FACE_OUTER_BOUND('',#1215,.T.);
#798=FACE_OUTER_BOUND('',#1216,.T.);
#799=FACE_OUTER_BOUND('',#1217,.T.);
#800=FACE_OUTER_BOUND('',#1218,.T.);
#801=FACE_OUTER_BOUND('',#1219,.T.);
#802=FACE_OUTER_BOUND('',#1220,.T.);
#803=FACE_OUTER_BOUND('',#1221,.T.);
#804=FACE_OUTER_BOUND('',#1222,.T.);
#805=FACE_OUTER_BOUND('',#1223,.T.);
#806=FACE_OUTER_BOUND('',#1224,.T.);
#807=FACE_OUTER_BOUND('',#1225,.T.);
#808=FACE_OUTER_BOUND('',#1226,.T.);
#809=FACE_OUTER_BOUND('',#1227,.T.);
#810=FACE_OUTER_BOUND('',#1228,.T.);
#811=FACE_OUTER_BOUND('',#1229,.T.);
#812=FACE_OUTER_BOUND('',#1230,.T.);
#813=FACE_OUTER_BOUND('',#1231,.T.);
#814=FACE_OUTER_BOUND('',#1232,.T.);
#815=FACE_OUTER_BOUND('',#1233,.T.);
#816=EDGE_LOOP('',(#3716,#3717,#3718,#3719));
#817=EDGE_LOOP('',(#3720,#3721,#3722,#3723));
#818=EDGE_LOOP('',(#3724,#3725,#3726,#3727));
#819=EDGE_LOOP('',(#3728,#3729,#3730,#3731));
#820=EDGE_LOOP('',(#3732,#3733,#3734,#3735));
#821=EDGE_LOOP('',(#3736,#3737,#3738,#3739));
#822=EDGE_LOOP('',(#3740,#3741,#3742,#3743));
#823=EDGE_LOOP('',(#3744,#3745,#3746,#3747));
#824=EDGE_LOOP('',(#3748,#3749,#3750,#3751));
#825=EDGE_LOOP('',(#3752,#3753,#3754,#3755));
#826=EDGE_LOOP('',(#3756,#3757,#3758,#3759,#3760,#3761,#3762,#3763));
#827=EDGE_LOOP('',(#3764));
#828=EDGE_LOOP('',(#3765));
#829=EDGE_LOOP('',(#3766));
#830=EDGE_LOOP('',(#3767));
#831=EDGE_LOOP('',(#3768));
#832=EDGE_LOOP('',(#3769));
#833=EDGE_LOOP('',(#3770));
#834=EDGE_LOOP('',(#3771));
#835=EDGE_LOOP('',(#3772,#3773,#3774,#3775));
#836=EDGE_LOOP('',(#3776,#3777,#3778,#3779));
#837=EDGE_LOOP('',(#3780,#3781,#3782,#3783));
#838=EDGE_LOOP('',(#3784,#3785,#3786,#3787));
#839=EDGE_LOOP('',(#3788,#3789,#3790,#3791));
#840=EDGE_LOOP('',(#3792,#3793,#3794,#3795));
#841=EDGE_LOOP('',(#3796,#3797,#3798,#3799,#3800,#3801,#3802,#3803));
#842=EDGE_LOOP('',(#3804));
#843=EDGE_LOOP('',(#3805));
#844=EDGE_LOOP('',(#3806));
#845=EDGE_LOOP('',(#3807));
#846=EDGE_LOOP('',(#3808));
#847=EDGE_LOOP('',(#3809));
#848=EDGE_LOOP('',(#3810));
#849=EDGE_LOOP('',(#3811));
#850=EDGE_LOOP('',(#3812,#3813,#3814,#3815));
#851=EDGE_LOOP('',(#3816,#3817,#3818,#3819));
#852=EDGE_LOOP('',(#3820,#3821,#3822,#3823));
#853=EDGE_LOOP('',(#3824,#3825,#3826,#3827));
#854=EDGE_LOOP('',(#3828,#3829,#3830,#3831));
#855=EDGE_LOOP('',(#3832,#3833,#3834,#3835));
#856=EDGE_LOOP('',(#3836,#3837,#3838,#3839));
#857=EDGE_LOOP('',(#3840,#3841,#3842,#3843));
#858=EDGE_LOOP('',(#3844,#3845,#3846,#3847));
#859=EDGE_LOOP('',(#3848,#3849,#3850,#3851));
#860=EDGE_LOOP('',(#3852,#3853,#3854,#3855));
#861=EDGE_LOOP('',(#3856,#3857,#3858,#3859));
#862=EDGE_LOOP('',(#3860,#3861,#3862,#3863));
#863=EDGE_LOOP('',(#3864,#3865,#3866,#3867));
#864=EDGE_LOOP('',(#3868,#3869,#3870,#3871));
#865=EDGE_LOOP('',(#3872,#3873,#3874,#3875));
#866=EDGE_LOOP('',(#3876,#3877,#3878,#3879));
#867=EDGE_LOOP('',(#3880,#3881,#3882,#3883));
#868=EDGE_LOOP('',(#3884,#3885,#3886,#3887));
#869=EDGE_LOOP('',(#3888,#3889,#3890,#3891,#3892,#3893,#3894,#3895,#3896,
#3897,#3898,#3899));
#870=EDGE_LOOP('',(#3900));
#871=EDGE_LOOP('',(#3901,#3902,#3903,#3904));
#872=EDGE_LOOP('',(#3905,#3906,#3907,#3908));
#873=EDGE_LOOP('',(#3909,#3910,#3911,#3912,#3913,#3914,#3915,#3916,#3917,
#3918,#3919,#3920));
#874=EDGE_LOOP('',(#3921));
#875=EDGE_LOOP('',(#3922,#3923,#3924,#3925));
#876=EDGE_LOOP('',(#3926,#3927,#3928,#3929));
#877=EDGE_LOOP('',(#3930,#3931,#3932,#3933));
#878=EDGE_LOOP('',(#3934,#3935,#3936,#3937));
#879=EDGE_LOOP('',(#3938,#3939,#3940,#3941));
#880=EDGE_LOOP('',(#3942,#3943,#3944,#3945));
#881=EDGE_LOOP('',(#3946,#3947,#3948,#3949));
#882=EDGE_LOOP('',(#3950,#3951,#3952,#3953,#3954,#3955));
#883=EDGE_LOOP('',(#3956,#3957,#3958,#3959));
#884=EDGE_LOOP('',(#3960,#3961,#3962,#3963));
#885=EDGE_LOOP('',(#3964,#3965,#3966,#3967));
#886=EDGE_LOOP('',(#3968,#3969,#3970,#3971,#3972,#3973));
#887=EDGE_LOOP('',(#3974,#3975,#3976,#3977));
#888=EDGE_LOOP('',(#3978,#3979,#3980,#3981));
#889=EDGE_LOOP('',(#3982,#3983,#3984,#3985));
#890=EDGE_LOOP('',(#3986,#3987,#3988,#3989));
#891=EDGE_LOOP('',(#3990,#3991,#3992,#3993));
#892=EDGE_LOOP('',(#3994,#3995,#3996,#3997));
#893=EDGE_LOOP('',(#3998,#3999,#4000,#4001));
#894=EDGE_LOOP('',(#4002,#4003,#4004,#4005,#4006,#4007));
#895=EDGE_LOOP('',(#4008));
#896=EDGE_LOOP('',(#4009));
#897=EDGE_LOOP('',(#4010,#4011,#4012,#4013,#4014,#4015,#4016,#4017,#4018,
#4019));
#898=EDGE_LOOP('',(#4020));
#899=EDGE_LOOP('',(#4021));
#900=EDGE_LOOP('',(#4022,#4023,#4024,#4025));
#901=EDGE_LOOP('',(#4026,#4027,#4028,#4029));
#902=EDGE_LOOP('',(#4030,#4031,#4032,#4033));
#903=EDGE_LOOP('',(#4034,#4035,#4036,#4037));
#904=EDGE_LOOP('',(#4038,#4039,#4040,#4041));
#905=EDGE_LOOP('',(#4042,#4043,#4044,#4045));
#906=EDGE_LOOP('',(#4046,#4047,#4048,#4049));
#907=EDGE_LOOP('',(#4050,#4051,#4052,#4053));
#908=EDGE_LOOP('',(#4054,#4055,#4056,#4057));
#909=EDGE_LOOP('',(#4058,#4059,#4060,#4061));
#910=EDGE_LOOP('',(#4062,#4063,#4064,#4065));
#911=EDGE_LOOP('',(#4066,#4067,#4068,#4069));
#912=EDGE_LOOP('',(#4070,#4071,#4072,#4073));
#913=EDGE_LOOP('',(#4074,#4075,#4076,#4077));
#914=EDGE_LOOP('',(#4078,#4079,#4080,#4081));
#915=EDGE_LOOP('',(#4082,#4083,#4084,#4085));
#916=EDGE_LOOP('',(#4086,#4087,#4088,#4089));
#917=EDGE_LOOP('',(#4090,#4091,#4092,#4093));
#918=EDGE_LOOP('',(#4094,#4095,#4096,#4097));
#919=EDGE_LOOP('',(#4098,#4099,#4100,#4101));
#920=EDGE_LOOP('',(#4102,#4103,#4104,#4105,#4106,#4107,#4108,#4109,#4110,
#4111,#4112,#4113));
#921=EDGE_LOOP('',(#4114));
#922=EDGE_LOOP('',(#4115));
#923=EDGE_LOOP('',(#4116));
#924=EDGE_LOOP('',(#4117));
#925=EDGE_LOOP('',(#4118,#4119,#4120,#4121));
#926=EDGE_LOOP('',(#4122,#4123,#4124,#4125));
#927=EDGE_LOOP('',(#4126,#4127,#4128,#4129));
#928=EDGE_LOOP('',(#4130,#4131,#4132,#4133));
#929=EDGE_LOOP('',(#4134,#4135,#4136,#4137));
#930=EDGE_LOOP('',(#4138,#4139,#4140,#4141));
#931=EDGE_LOOP('',(#4142,#4143,#4144,#4145));
#932=EDGE_LOOP('',(#4146,#4147,#4148,#4149));
#933=EDGE_LOOP('',(#4150,#4151,#4152,#4153));
#934=EDGE_LOOP('',(#4154,#4155,#4156,#4157));
#935=EDGE_LOOP('',(#4158,#4159,#4160,#4161,#4162,#4163,#4164,#4165,#4166,
#4167));
#936=EDGE_LOOP('',(#4168,#4169,#4170,#4171));
#937=EDGE_LOOP('',(#4172,#4173,#4174,#4175));
#938=EDGE_LOOP('',(#4176,#4177,#4178,#4179));
#939=EDGE_LOOP('',(#4180,#4181,#4182,#4183,#4184,#4185,#4186,#4187,#4188,
#4189));
#940=EDGE_LOOP('',(#4190,#4191,#4192,#4193));
#941=EDGE_LOOP('',(#4194,#4195,#4196,#4197));
#942=EDGE_LOOP('',(#4198,#4199,#4200,#4201));
#943=EDGE_LOOP('',(#4202,#4203,#4204,#4205));
#944=EDGE_LOOP('',(#4206,#4207,#4208,#4209));
#945=EDGE_LOOP('',(#4210,#4211,#4212,#4213));
#946=EDGE_LOOP('',(#4214,#4215,#4216,#4217));
#947=EDGE_LOOP('',(#4218,#4219,#4220,#4221));
#948=EDGE_LOOP('',(#4222,#4223,#4224,#4225));
#949=EDGE_LOOP('',(#4226,#4227,#4228,#4229));
#950=EDGE_LOOP('',(#4230,#4231,#4232,#4233));
#951=EDGE_LOOP('',(#4234,#4235,#4236,#4237));
#952=EDGE_LOOP('',(#4238,#4239,#4240,#4241));
#953=EDGE_LOOP('',(#4242,#4243,#4244,#4245));
#954=EDGE_LOOP('',(#4246,#4247,#4248,#4249));
#955=EDGE_LOOP('',(#4250,#4251,#4252,#4253));
#956=EDGE_LOOP('',(#4254,#4255,#4256,#4257));
#957=EDGE_LOOP('',(#4258,#4259,#4260,#4261));
#958=EDGE_LOOP('',(#4262,#4263,#4264,#4265));
#959=EDGE_LOOP('',(#4266,#4267,#4268,#4269,#4270,#4271,#4272,#4273,#4274,
#4275,#4276,#4277));
#960=EDGE_LOOP('',(#4278,#4279,#4280,#4281));
#961=EDGE_LOOP('',(#4282,#4283,#4284,#4285));
#962=EDGE_LOOP('',(#4286,#4287,#4288,#4289));
#963=EDGE_LOOP('',(#4290,#4291,#4292,#4293));
#964=EDGE_LOOP('',(#4294,#4295,#4296,#4297));
#965=EDGE_LOOP('',(#4298,#4299,#4300,#4301));
#966=EDGE_LOOP('',(#4302,#4303,#4304,#4305));
#967=EDGE_LOOP('',(#4306,#4307,#4308,#4309));
#968=EDGE_LOOP('',(#4310,#4311,#4312,#4313));
#969=EDGE_LOOP('',(#4314,#4315,#4316,#4317));
#970=EDGE_LOOP('',(#4318,#4319,#4320,#4321));
#971=EDGE_LOOP('',(#4322,#4323,#4324,#4325));
#972=EDGE_LOOP('',(#4326,#4327,#4328,#4329));
#973=EDGE_LOOP('',(#4330,#4331,#4332,#4333));
#974=EDGE_LOOP('',(#4334,#4335,#4336,#4337));
#975=EDGE_LOOP('',(#4338,#4339,#4340,#4341,#4342,#4343,#4344,#4345,#4346,
#4347,#4348,#4349));
#976=EDGE_LOOP('',(#4350,#4351,#4352,#4353));
#977=EDGE_LOOP('',(#4354,#4355,#4356,#4357));
#978=EDGE_LOOP('',(#4358,#4359,#4360,#4361));
#979=EDGE_LOOP('',(#4362,#4363,#4364,#4365));
#980=EDGE_LOOP('',(#4366,#4367,#4368,#4369));
#981=EDGE_LOOP('',(#4370,#4371,#4372,#4373));
#982=EDGE_LOOP('',(#4374,#4375,#4376,#4377));
#983=EDGE_LOOP('',(#4378,#4379,#4380,#4381));
#984=EDGE_LOOP('',(#4382,#4383,#4384,#4385));
#985=EDGE_LOOP('',(#4386,#4387,#4388,#4389));
#986=EDGE_LOOP('',(#4390,#4391,#4392,#4393));
#987=EDGE_LOOP('',(#4394,#4395,#4396,#4397));
#988=EDGE_LOOP('',(#4398,#4399,#4400,#4401));
#989=EDGE_LOOP('',(#4402,#4403,#4404,#4405));
#990=EDGE_LOOP('',(#4406,#4407,#4408,#4409));
#991=EDGE_LOOP('',(#4410,#4411,#4412,#4413));
#992=EDGE_LOOP('',(#4414,#4415,#4416,#4417));
#993=EDGE_LOOP('',(#4418,#4419,#4420,#4421));
#994=EDGE_LOOP('',(#4422,#4423,#4424,#4425));
#995=EDGE_LOOP('',(#4426,#4427,#4428,#4429));
#996=EDGE_LOOP('',(#4430,#4431,#4432,#4433));
#997=EDGE_LOOP('',(#4434,#4435,#4436,#4437));
#998=EDGE_LOOP('',(#4438,#4439,#4440,#4441));
#999=EDGE_LOOP('',(#4442,#4443,#4444,#4445));
#1000=EDGE_LOOP('',(#4446,#4447,#4448,#4449));
#1001=EDGE_LOOP('',(#4450,#4451,#4452,#4453,#4454,#4455,#4456,#4457));
#1002=EDGE_LOOP('',(#4458));
#1003=EDGE_LOOP('',(#4459));
#1004=EDGE_LOOP('',(#4460));
#1005=EDGE_LOOP('',(#4461));
#1006=EDGE_LOOP('',(#4462));
#1007=EDGE_LOOP('',(#4463));
#1008=EDGE_LOOP('',(#4464));
#1009=EDGE_LOOP('',(#4465));
#1010=EDGE_LOOP('',(#4466));
#1011=EDGE_LOOP('',(#4467));
#1012=EDGE_LOOP('',(#4468,#4469,#4470,#4471));
#1013=EDGE_LOOP('',(#4472,#4473,#4474,#4475));
#1014=EDGE_LOOP('',(#4476,#4477,#4478,#4479));
#1015=EDGE_LOOP('',(#4480,#4481,#4482,#4483));
#1016=EDGE_LOOP('',(#4484,#4485,#4486,#4487));
#1017=EDGE_LOOP('',(#4488,#4489,#4490,#4491));
#1018=EDGE_LOOP('',(#4492,#4493,#4494,#4495));
#1019=EDGE_LOOP('',(#4496,#4497,#4498,#4499));
#1020=EDGE_LOOP('',(#4500,#4501,#4502,#4503));
#1021=EDGE_LOOP('',(#4504,#4505,#4506,#4507));
#1022=EDGE_LOOP('',(#4508,#4509,#4510,#4511));
#1023=EDGE_LOOP('',(#4512,#4513,#4514,#4515,#4516,#4517,#4518,#4519));
#1024=EDGE_LOOP('',(#4520));
#1025=EDGE_LOOP('',(#4521));
#1026=EDGE_LOOP('',(#4522));
#1027=EDGE_LOOP('',(#4523));
#1028=EDGE_LOOP('',(#4524));
#1029=EDGE_LOOP('',(#4525));
#1030=EDGE_LOOP('',(#4526));
#1031=EDGE_LOOP('',(#4527));
#1032=EDGE_LOOP('',(#4528));
#1033=EDGE_LOOP('',(#4529));
#1034=EDGE_LOOP('',(#4530,#4531,#4532,#4533));
#1035=EDGE_LOOP('',(#4534,#4535,#4536,#4537));
#1036=EDGE_LOOP('',(#4538,#4539,#4540,#4541));
#1037=EDGE_LOOP('',(#4542,#4543,#4544,#4545,#4546,#4547,#4548,#4549));
#1038=EDGE_LOOP('',(#4550,#4551,#4552,#4553));
#1039=EDGE_LOOP('',(#4554,#4555,#4556,#4557));
#1040=EDGE_LOOP('',(#4558));
#1041=EDGE_LOOP('',(#4559,#4560,#4561,#4562));
#1042=EDGE_LOOP('',(#4563,#4564,#4565,#4566));
#1043=EDGE_LOOP('',(#4567));
#1044=EDGE_LOOP('',(#4568));
#1045=EDGE_LOOP('',(#4569,#4570,#4571,#4572));
#1046=EDGE_LOOP('',(#4573,#4574,#4575,#4576));
#1047=EDGE_LOOP('',(#4577));
#1048=EDGE_LOOP('',(#4578,#4579,#4580,#4581));
#1049=EDGE_LOOP('',(#4582,#4583,#4584,#4585));
#1050=EDGE_LOOP('',(#4586,#4587,#4588,#4589,#4590,#4591,#4592,#4593));
#1051=EDGE_LOOP('',(#4594,#4595,#4596,#4597));
#1052=EDGE_LOOP('',(#4598));
#1053=EDGE_LOOP('',(#4599,#4600,#4601,#4602));
#1054=EDGE_LOOP('',(#4603));
#1055=EDGE_LOOP('',(#4604,#4605,#4606,#4607));
#1056=EDGE_LOOP('',(#4608));
#1057=EDGE_LOOP('',(#4609,#4610,#4611,#4612));
#1058=EDGE_LOOP('',(#4613,#4614,#4615,#4616));
#1059=EDGE_LOOP('',(#4617,#4618,#4619,#4620));
#1060=EDGE_LOOP('',(#4621,#4622,#4623,#4624));
#1061=EDGE_LOOP('',(#4625,#4626,#4627,#4628,#4629,#4630));
#1062=EDGE_LOOP('',(#4631,#4632,#4633,#4634,#4635,#4636,#4637,#4638,#4639,
#4640,#4641,#4642));
#1063=EDGE_LOOP('',(#4643,#4644,#4645,#4646));
#1064=EDGE_LOOP('',(#4647));
#1065=EDGE_LOOP('',(#4648));
#1066=EDGE_LOOP('',(#4649));
#1067=EDGE_LOOP('',(#4650,#4651,#4652,#4653,#4654,#4655));
#1068=EDGE_LOOP('',(#4656,#4657,#4658,#4659,#4660,#4661,#4662,#4663,#4664,
#4665,#4666,#4667));
#1069=EDGE_LOOP('',(#4668,#4669,#4670,#4671));
#1070=EDGE_LOOP('',(#4672,#4673,#4674,#4675));
#1071=EDGE_LOOP('',(#4676,#4677,#4678,#4679));
#1072=EDGE_LOOP('',(#4680,#4681,#4682,#4683));
#1073=EDGE_LOOP('',(#4684,#4685,#4686,#4687));
#1074=EDGE_LOOP('',(#4688,#4689,#4690,#4691));
#1075=EDGE_LOOP('',(#4692,#4693,#4694,#4695));
#1076=EDGE_LOOP('',(#4696,#4697,#4698,#4699));
#1077=EDGE_LOOP('',(#4700,#4701,#4702,#4703));
#1078=EDGE_LOOP('',(#4704,#4705,#4706,#4707));
#1079=EDGE_LOOP('',(#4708,#4709,#4710,#4711));
#1080=EDGE_LOOP('',(#4712,#4713,#4714,#4715));
#1081=EDGE_LOOP('',(#4716,#4717,#4718,#4719));
#1082=EDGE_LOOP('',(#4720,#4721,#4722,#4723));
#1083=EDGE_LOOP('',(#4724,#4725,#4726,#4727));
#1084=EDGE_LOOP('',(#4728,#4729,#4730,#4731));
#1085=EDGE_LOOP('',(#4732,#4733,#4734,#4735));
#1086=EDGE_LOOP('',(#4736,#4737,#4738,#4739));
#1087=EDGE_LOOP('',(#4740,#4741,#4742,#4743));
#1088=EDGE_LOOP('',(#4744,#4745,#4746,#4747));
#1089=EDGE_LOOP('',(#4748,#4749,#4750,#4751));
#1090=EDGE_LOOP('',(#4752,#4753,#4754,#4755));
#1091=EDGE_LOOP('',(#4756,#4757,#4758,#4759));
#1092=EDGE_LOOP('',(#4760,#4761,#4762,#4763));
#1093=EDGE_LOOP('',(#4764,#4765,#4766,#4767));
#1094=EDGE_LOOP('',(#4768,#4769,#4770,#4771));
#1095=EDGE_LOOP('',(#4772,#4773,#4774,#4775));
#1096=EDGE_LOOP('',(#4776,#4777,#4778,#4779));
#1097=EDGE_LOOP('',(#4780,#4781,#4782,#4783));
#1098=EDGE_LOOP('',(#4784,#4785,#4786,#4787));
#1099=EDGE_LOOP('',(#4788,#4789,#4790,#4791));
#1100=EDGE_LOOP('',(#4792,#4793,#4794,#4795));
#1101=EDGE_LOOP('',(#4796,#4797,#4798,#4799));
#1102=EDGE_LOOP('',(#4800,#4801,#4802,#4803));
#1103=EDGE_LOOP('',(#4804,#4805,#4806,#4807));
#1104=EDGE_LOOP('',(#4808,#4809,#4810,#4811));
#1105=EDGE_LOOP('',(#4812,#4813,#4814,#4815));
#1106=EDGE_LOOP('',(#4816,#4817,#4818,#4819));
#1107=EDGE_LOOP('',(#4820,#4821,#4822,#4823));
#1108=EDGE_LOOP('',(#4824,#4825,#4826,#4827));
#1109=EDGE_LOOP('',(#4828,#4829,#4830,#4831));
#1110=EDGE_LOOP('',(#4832,#4833,#4834,#4835));
#1111=EDGE_LOOP('',(#4836,#4837,#4838,#4839));
#1112=EDGE_LOOP('',(#4840,#4841,#4842,#4843));
#1113=EDGE_LOOP('',(#4844,#4845,#4846,#4847));
#1114=EDGE_LOOP('',(#4848,#4849,#4850,#4851));
#1115=EDGE_LOOP('',(#4852,#4853,#4854,#4855));
#1116=EDGE_LOOP('',(#4856,#4857,#4858,#4859));
#1117=EDGE_LOOP('',(#4860,#4861,#4862,#4863));
#1118=EDGE_LOOP('',(#4864,#4865,#4866,#4867,#4868,#4869,#4870,#4871,#4872,
#4873,#4874,#4875));
#1119=EDGE_LOOP('',(#4876));
#1120=EDGE_LOOP('',(#4877));
#1121=EDGE_LOOP('',(#4878));
#1122=EDGE_LOOP('',(#4879));
#1123=EDGE_LOOP('',(#4880,#4881,#4882,#4883));
#1124=EDGE_LOOP('',(#4884,#4885,#4886,#4887));
#1125=EDGE_LOOP('',(#4888,#4889,#4890,#4891));
#1126=EDGE_LOOP('',(#4892,#4893,#4894,#4895));
#1127=EDGE_LOOP('',(#4896,#4897,#4898,#4899));
#1128=EDGE_LOOP('',(#4900,#4901,#4902,#4903));
#1129=EDGE_LOOP('',(#4904,#4905,#4906,#4907));
#1130=EDGE_LOOP('',(#4908,#4909,#4910,#4911));
#1131=EDGE_LOOP('',(#4912,#4913,#4914,#4915));
#1132=EDGE_LOOP('',(#4916,#4917,#4918,#4919));
#1133=EDGE_LOOP('',(#4920,#4921,#4922,#4923));
#1134=EDGE_LOOP('',(#4924,#4925,#4926,#4927));
#1135=EDGE_LOOP('',(#4928,#4929,#4930,#4931));
#1136=EDGE_LOOP('',(#4932,#4933,#4934,#4935));
#1137=EDGE_LOOP('',(#4936,#4937,#4938,#4939,#4940,#4941,#4942,#4943,#4944,
#4945,#4946,#4947));
#1138=EDGE_LOOP('',(#4948));
#1139=EDGE_LOOP('',(#4949));
#1140=EDGE_LOOP('',(#4950));
#1141=EDGE_LOOP('',(#4951));
#1142=EDGE_LOOP('',(#4952,#4953,#4954,#4955));
#1143=EDGE_LOOP('',(#4956,#4957,#4958,#4959));
#1144=EDGE_LOOP('',(#4960,#4961,#4962,#4963));
#1145=EDGE_LOOP('',(#4964,#4965,#4966,#4967));
#1146=EDGE_LOOP('',(#4968,#4969,#4970,#4971));
#1147=EDGE_LOOP('',(#4972,#4973,#4974,#4975));
#1148=EDGE_LOOP('',(#4976,#4977,#4978,#4979));
#1149=EDGE_LOOP('',(#4980,#4981,#4982,#4983));
#1150=EDGE_LOOP('',(#4984,#4985,#4986,#4987));
#1151=EDGE_LOOP('',(#4988,#4989,#4990,#4991));
#1152=EDGE_LOOP('',(#4992,#4993,#4994,#4995));
#1153=EDGE_LOOP('',(#4996,#4997,#4998,#4999));
#1154=EDGE_LOOP('',(#5000,#5001,#5002,#5003));
#1155=EDGE_LOOP('',(#5004,#5005,#5006,#5007));
#1156=EDGE_LOOP('',(#5008,#5009,#5010,#5011));
#1157=EDGE_LOOP('',(#5012,#5013,#5014,#5015));
#1158=EDGE_LOOP('',(#5016,#5017,#5018,#5019));
#1159=EDGE_LOOP('',(#5020,#5021,#5022,#5023));
#1160=EDGE_LOOP('',(#5024,#5025,#5026,#5027));
#1161=EDGE_LOOP('',(#5028,#5029,#5030,#5031));
#1162=EDGE_LOOP('',(#5032,#5033,#5034,#5035));
#1163=EDGE_LOOP('',(#5036,#5037,#5038,#5039));
#1164=EDGE_LOOP('',(#5040,#5041,#5042,#5043));
#1165=EDGE_LOOP('',(#5044,#5045,#5046,#5047));
#1166=EDGE_LOOP('',(#5048,#5049,#5050,#5051));
#1167=EDGE_LOOP('',(#5052,#5053,#5054,#5055));
#1168=EDGE_LOOP('',(#5056,#5057,#5058,#5059,#5060,#5061,#5062,#5063,#5064,
#5065,#5066,#5067));
#1169=EDGE_LOOP('',(#5068));
#1170=EDGE_LOOP('',(#5069));
#1171=EDGE_LOOP('',(#5070));
#1172=EDGE_LOOP('',(#5071));
#1173=EDGE_LOOP('',(#5072,#5073,#5074,#5075));
#1174=EDGE_LOOP('',(#5076,#5077,#5078,#5079));
#1175=EDGE_LOOP('',(#5080,#5081,#5082,#5083));
#1176=EDGE_LOOP('',(#5084,#5085,#5086,#5087));
#1177=EDGE_LOOP('',(#5088,#5089,#5090,#5091));
#1178=EDGE_LOOP('',(#5092,#5093,#5094,#5095));
#1179=EDGE_LOOP('',(#5096,#5097,#5098,#5099));
#1180=EDGE_LOOP('',(#5100,#5101,#5102,#5103));
#1181=EDGE_LOOP('',(#5104,#5105,#5106,#5107));
#1182=EDGE_LOOP('',(#5108,#5109,#5110,#5111));
#1183=EDGE_LOOP('',(#5112,#5113,#5114,#5115));
#1184=EDGE_LOOP('',(#5116,#5117,#5118,#5119));
#1185=EDGE_LOOP('',(#5120,#5121,#5122,#5123));
#1186=EDGE_LOOP('',(#5124,#5125,#5126,#5127));
#1187=EDGE_LOOP('',(#5128,#5129,#5130,#5131,#5132,#5133,#5134,#5135,#5136,
#5137,#5138,#5139));
#1188=EDGE_LOOP('',(#5140));
#1189=EDGE_LOOP('',(#5141));
#1190=EDGE_LOOP('',(#5142));
#1191=EDGE_LOOP('',(#5143));
#1192=EDGE_LOOP('',(#5144,#5145,#5146,#5147));
#1193=EDGE_LOOP('',(#5148,#5149,#5150,#5151));
#1194=EDGE_LOOP('',(#5152,#5153,#5154,#5155));
#1195=EDGE_LOOP('',(#5156,#5157,#5158,#5159));
#1196=EDGE_LOOP('',(#5160,#5161,#5162,#5163));
#1197=EDGE_LOOP('',(#5164,#5165,#5166,#5167));
#1198=EDGE_LOOP('',(#5168,#5169,#5170,#5171));
#1199=EDGE_LOOP('',(#5172,#5173,#5174,#5175));
#1200=EDGE_LOOP('',(#5176,#5177,#5178,#5179));
#1201=EDGE_LOOP('',(#5180,#5181,#5182,#5183));
#1202=EDGE_LOOP('',(#5184,#5185,#5186,#5187));
#1203=EDGE_LOOP('',(#5188,#5189,#5190,#5191));
#1204=EDGE_LOOP('',(#5192,#5193,#5194,#5195));
#1205=EDGE_LOOP('',(#5196,#5197,#5198,#5199));
#1206=EDGE_LOOP('',(#5200,#5201,#5202,#5203));
#1207=EDGE_LOOP('',(#5204,#5205,#5206,#5207));
#1208=EDGE_LOOP('',(#5208,#5209,#5210,#5211));
#1209=EDGE_LOOP('',(#5212,#5213,#5214,#5215));
#1210=EDGE_LOOP('',(#5216,#5217,#5218,#5219));
#1211=EDGE_LOOP('',(#5220,#5221,#5222,#5223));
#1212=EDGE_LOOP('',(#5224,#5225,#5226,#5227));
#1213=EDGE_LOOP('',(#5228,#5229,#5230,#5231));
#1214=EDGE_LOOP('',(#5232,#5233,#5234,#5235,#5236,#5237,#5238,#5239,#5240,
#5241,#5242,#5243));
#1215=EDGE_LOOP('',(#5244,#5245,#5246,#5247));
#1216=EDGE_LOOP('',(#5248,#5249,#5250,#5251));
#1217=EDGE_LOOP('',(#5252,#5253,#5254,#5255));
#1218=EDGE_LOOP('',(#5256,#5257,#5258,#5259));
#1219=EDGE_LOOP('',(#5260,#5261,#5262,#5263));
#1220=EDGE_LOOP('',(#5264,#5265,#5266,#5267));
#1221=EDGE_LOOP('',(#5268,#5269,#5270,#5271));
#1222=EDGE_LOOP('',(#5272,#5273,#5274,#5275));
#1223=EDGE_LOOP('',(#5276,#5277,#5278,#5279));
#1224=EDGE_LOOP('',(#5280,#5281,#5282,#5283));
#1225=EDGE_LOOP('',(#5284,#5285,#5286,#5287));
#1226=EDGE_LOOP('',(#5288,#5289,#5290,#5291));
#1227=EDGE_LOOP('',(#5292,#5293,#5294,#5295));
#1228=EDGE_LOOP('',(#5296,#5297,#5298,#5299));
#1229=EDGE_LOOP('',(#5300,#5301,#5302,#5303));
#1230=EDGE_LOOP('',(#5304,#5305,#5306,#5307,#5308,#5309,#5310,#5311,#5312,
#5313,#5314,#5315));
#1231=EDGE_LOOP('',(#5316,#5317,#5318,#5319));
#1232=EDGE_LOOP('',(#5320,#5321,#5322,#5323));
#1233=EDGE_LOOP('',(#5324,#5325,#5326,#5327));
#1234=LINE('',#8422,#1784);
#1235=LINE('',#8428,#1785);
#1236=LINE('',#8434,#1786);
#1237=LINE('',#8440,#1787);
#1238=LINE('',#8446,#1788);
#1239=LINE('',#8452,#1789);
#1240=LINE('',#8458,#1790);
#1241=LINE('',#8464,#1791);
#1242=LINE('',#8471,#1792);
#1243=LINE('',#8474,#1793);
#1244=LINE('',#8477,#1794);
#1245=LINE('',#8479,#1795);
#1246=LINE('',#8480,#1796);
#1247=LINE('',#8483,#1797);
#1248=LINE('',#8487,#1798);
#1249=LINE('',#8491,#1799);
#1250=LINE('',#8497,#1800);
#1251=LINE('',#8498,#1801);
#1252=LINE('',#8501,#1802);
#1253=LINE('',#8502,#1803);
#1254=LINE('',#8506,#1804);
#1255=LINE('',#8510,#1805);
#1256=LINE('',#8512,#1806);
#1257=LINE('',#8514,#1807);
#1258=LINE('',#8521,#1808);
#1259=LINE('',#8526,#1809);
#1260=LINE('',#8528,#1810);
#1261=LINE('',#8530,#1811);
#1262=LINE('',#8531,#1812);
#1263=LINE('',#8534,#1813);
#1264=LINE('',#8536,#1814);
#1265=LINE('',#8537,#1815);
#1266=LINE('',#8540,#1816);
#1267=LINE('',#8542,#1817);
#1268=LINE('',#8543,#1818);
#1269=LINE('',#8546,#1819);
#1270=LINE('',#8548,#1820);
#1271=LINE('',#8549,#1821);
#1272=LINE('',#8552,#1822);
#1273=LINE('',#8554,#1823);
#1274=LINE('',#8555,#1824);
#1275=LINE('',#8558,#1825);
#1276=LINE('',#8560,#1826);
#1277=LINE('',#8561,#1827);
#1278=LINE('',#8564,#1828);
#1279=LINE('',#8566,#1829);
#1280=LINE('',#8567,#1830);
#1281=LINE('',#8570,#1831);
#1282=LINE('',#8572,#1832);
#1283=LINE('',#8573,#1833);
#1284=LINE('',#8576,#1834);
#1285=LINE('',#8578,#1835);
#1286=LINE('',#8579,#1836);
#1287=LINE('',#8582,#1837);
#1288=LINE('',#8584,#1838);
#1289=LINE('',#8585,#1839);
#1290=LINE('',#8588,#1840);
#1291=LINE('',#8590,#1841);
#1292=LINE('',#8591,#1842);
#1293=LINE('',#8593,#1843);
#1294=LINE('',#8594,#1844);
#1295=LINE('',#8597,#1845);
#1296=LINE('',#8599,#1846);
#1297=LINE('',#8600,#1847);
#1298=LINE('',#8603,#1848);
#1299=LINE('',#8604,#1849);
#1300=LINE('',#8607,#1850);
#1301=LINE('',#8608,#1851);
#1302=LINE('',#8611,#1852);
#1303=LINE('',#8612,#1853);
#1304=LINE('',#8615,#1854);
#1305=LINE('',#8616,#1855);
#1306=LINE('',#8619,#1856);
#1307=LINE('',#8620,#1857);
#1308=LINE('',#8624,#1858);
#1309=LINE('',#8626,#1859);
#1310=LINE('',#8627,#1860);
#1311=LINE('',#8630,#1861);
#1312=LINE('',#8631,#1862);
#1313=LINE('',#8633,#1863);
#1314=LINE('',#8635,#1864);
#1315=LINE('',#8637,#1865);
#1316=LINE('',#8638,#1866);
#1317=LINE('',#8640,#1867);
#1318=LINE('',#8642,#1868);
#1319=LINE('',#8668,#1869);
#1320=LINE('',#8669,#1870);
#1321=LINE('',#8687,#1871);
#1322=LINE('',#8689,#1872);
#1323=LINE('',#8690,#1873);
#1324=LINE('',#8713,#1874);
#1325=LINE('',#8714,#1875);
#1326=LINE('',#8732,#1876);
#1327=LINE('',#8734,#1877);
#1328=LINE('',#8735,#1878);
#1329=LINE('',#8740,#1879);
#1330=LINE('',#8746,#1880);
#1331=LINE('',#8752,#1881);
#1332=LINE('',#8758,#1882);
#1333=LINE('',#8761,#1883);
#1334=LINE('',#8762,#1884);
#1335=LINE('',#8765,#1885);
#1336=LINE('',#8768,#1886);
#1337=LINE('',#8771,#1887);
#1338=LINE('',#8774,#1888);
#1339=LINE('',#8777,#1889);
#1340=LINE('',#8779,#1890);
#1341=LINE('',#8781,#1891);
#1342=LINE('',#8782,#1892);
#1343=LINE('',#8785,#1893);
#1344=LINE('',#8787,#1894);
#1345=LINE('',#8789,#1895);
#1346=LINE('',#8791,#1896);
#1347=LINE('',#8793,#1897);
#1348=LINE('',#8795,#1898);
#1349=LINE('',#8797,#1899);
#1350=LINE('',#8798,#1900);
#1351=LINE('',#8802,#1901);
#1352=LINE('',#8805,#1902);
#1353=LINE('',#8810,#1903);
#1354=LINE('',#8814,#1904);
#1355=LINE('',#8819,#1905);
#1356=LINE('',#8823,#1906);
#1357=LINE('',#8827,#1907);
#1358=LINE('',#8830,#1908);
#1359=LINE('',#8834,#1909);
#1360=LINE('',#8838,#1910);
#1361=LINE('',#8842,#1911);
#1362=LINE('',#8845,#1912);
#1363=LINE('',#8847,#1913);
#1364=LINE('',#8848,#1914);
#1365=LINE('',#8851,#1915);
#1366=LINE('',#8853,#1916);
#1367=LINE('',#8857,#1917);
#1368=LINE('',#8859,#1918);
#1369=LINE('',#8862,#1919);
#1370=LINE('',#8863,#1920);
#1371=LINE('',#8866,#1921);
#1372=LINE('',#8868,#1922);
#1373=LINE('',#8872,#1923);
#1374=LINE('',#8874,#1924);
#1375=LINE('',#8877,#1925);
#1376=LINE('',#8878,#1926);
#1377=LINE('',#8881,#1927);
#1378=LINE('',#8882,#1928);
#1379=LINE('',#8883,#1929);
#1380=LINE('',#8886,#1930);
#1381=LINE('',#8887,#1931);
#1382=LINE('',#8890,#1932);
#1383=LINE('',#8891,#1933);
#1384=LINE('',#8894,#1934);
#1385=LINE('',#8895,#1935);
#1386=LINE('',#8898,#1936);
#1387=LINE('',#8899,#1937);
#1388=LINE('',#8902,#1938);
#1389=LINE('',#8903,#1939);
#1390=LINE('',#8908,#1940);
#1391=LINE('',#8912,#1941);
#1392=LINE('',#8914,#1942);
#1393=LINE('',#8917,#1943);
#1394=LINE('',#8930,#1944);
#1395=LINE('',#8932,#1945);
#1396=LINE('',#8934,#1946);
#1397=LINE('',#8936,#1947);
#1398=LINE('',#8938,#1948);
#1399=LINE('',#8944,#1949);
#1400=LINE('',#8948,#1950);
#1401=LINE('',#8953,#1951);
#1402=LINE('',#8957,#1952);
#1403=LINE('',#8961,#1953);
#1404=LINE('',#8964,#1954);
#1405=LINE('',#8967,#1955);
#1406=LINE('',#8970,#1956);
#1407=LINE('',#8973,#1957);
#1408=LINE('',#8976,#1958);
#1409=LINE('',#8979,#1959);
#1410=LINE('',#8982,#1960);
#1411=LINE('',#8985,#1961);
#1412=LINE('',#8987,#1962);
#1413=LINE('',#8991,#1963);
#1414=LINE('',#8993,#1964);
#1415=LINE('',#8997,#1965);
#1416=LINE('',#8999,#1966);
#1417=LINE('',#9003,#1967);
#1418=LINE('',#9005,#1968);
#1419=LINE('',#9008,#1969);
#1420=LINE('',#9009,#1970);
#1421=LINE('',#9011,#1971);
#1422=LINE('',#9012,#1972);
#1423=LINE('',#9015,#1973);
#1424=LINE('',#9017,#1974);
#1425=LINE('',#9018,#1975);
#1426=LINE('',#9021,#1976);
#1427=LINE('',#9022,#1977);
#1428=LINE('',#9025,#1978);
#1429=LINE('',#9026,#1979);
#1430=LINE('',#9029,#1980);
#1431=LINE('',#9030,#1981);
#1432=LINE('',#9033,#1982);
#1433=LINE('',#9034,#1983);
#1434=LINE('',#9037,#1984);
#1435=LINE('',#9038,#1985);
#1436=LINE('',#9043,#1986);
#1437=LINE('',#9048,#1987);
#1438=LINE('',#9052,#1988);
#1439=LINE('',#9056,#1989);
#1440=LINE('',#9060,#1990);
#1441=LINE('',#9063,#1991);
#1442=LINE('',#9066,#1992);
#1443=LINE('',#9068,#1993);
#1444=LINE('',#9072,#1994);
#1445=LINE('',#9074,#1995);
#1446=LINE('',#9078,#1996);
#1447=LINE('',#9080,#1997);
#1448=LINE('',#9084,#1998);
#1449=LINE('',#9086,#1999);
#1450=LINE('',#9089,#2000);
#1451=LINE('',#9091,#2001);
#1452=LINE('',#9095,#2002);
#1453=LINE('',#9098,#2003);
#1454=LINE('',#9100,#2004);
#1455=LINE('',#9101,#2005);
#1456=LINE('',#9103,#2006);
#1457=LINE('',#9107,#2007);
#1458=LINE('',#9108,#2008);
#1459=LINE('',#9116,#2009);
#1460=LINE('',#9122,#2010);
#1461=LINE('',#9128,#2011);
#1462=LINE('',#9134,#2012);
#1463=LINE('',#9140,#2013);
#1464=LINE('',#9146,#2014);
#1465=LINE('',#9152,#2015);
#1466=LINE('',#9158,#2016);
#1467=LINE('',#9164,#2017);
#1468=LINE('',#9170,#2018);
#1469=LINE('',#9175,#2019);
#1470=LINE('',#9179,#2020);
#1471=LINE('',#9183,#2021);
#1472=LINE('',#9186,#2022);
#1473=LINE('',#9189,#2023);
#1474=LINE('',#9192,#2024);
#1475=LINE('',#9195,#2025);
#1476=LINE('',#9198,#2026);
#1477=LINE('',#9201,#2027);
#1478=LINE('',#9203,#2028);
#1479=LINE('',#9207,#2029);
#1480=LINE('',#9209,#2030);
#1481=LINE('',#9213,#2031);
#1482=LINE('',#9215,#2032);
#1483=LINE('',#9218,#2033);
#1484=LINE('',#9219,#2034);
#1485=LINE('',#9222,#2035);
#1486=LINE('',#9224,#2036);
#1487=LINE('',#9225,#2037);
#1488=LINE('',#9228,#2038);
#1489=LINE('',#9229,#2039);
#1490=LINE('',#9232,#2040);
#1491=LINE('',#9233,#2041);
#1492=LINE('',#9236,#2042);
#1493=LINE('',#9237,#2043);
#1494=LINE('',#9242,#2044);
#1495=LINE('',#9247,#2045);
#1496=LINE('',#9251,#2046);
#1497=LINE('',#9255,#2047);
#1498=LINE('',#9259,#2048);
#1499=LINE('',#9261,#2049);
#1500=LINE('',#9265,#2050);
#1501=LINE('',#9267,#2051);
#1502=LINE('',#9271,#2052);
#1503=LINE('',#9273,#2053);
#1504=LINE('',#9276,#2054);
#1505=LINE('',#9277,#2055);
#1506=LINE('',#9279,#2056);
#1507=LINE('',#9280,#2057);
#1508=LINE('',#9282,#2058);
#1509=LINE('',#9291,#2059);
#1510=LINE('',#9297,#2060);
#1511=LINE('',#9302,#2061);
#1512=LINE('',#9304,#2062);
#1513=LINE('',#9306,#2063);
#1514=LINE('',#9308,#2064);
#1515=LINE('',#9310,#2065);
#1516=LINE('',#9312,#2066);
#1517=LINE('',#9314,#2067);
#1518=LINE('',#9315,#2068);
#1519=LINE('',#9318,#2069);
#1520=LINE('',#9320,#2070);
#1521=LINE('',#9321,#2071);
#1522=LINE('',#9324,#2072);
#1523=LINE('',#9325,#2073);
#1524=LINE('',#9328,#2074);
#1525=LINE('',#9329,#2075);
#1526=LINE('',#9332,#2076);
#1527=LINE('',#9333,#2077);
#1528=LINE('',#9336,#2078);
#1529=LINE('',#9337,#2079);
#1530=LINE('',#9340,#2080);
#1531=LINE('',#9341,#2081);
#1532=LINE('',#9344,#2082);
#1533=LINE('',#9345,#2083);
#1534=LINE('',#9347,#2084);
#1535=LINE('',#9354,#2085);
#1536=LINE('',#9361,#2086);
#1537=LINE('',#9368,#2087);
#1538=LINE('',#9374,#2088);
#1539=LINE('',#9378,#2089);
#1540=LINE('',#9382,#2090);
#1541=LINE('',#9384,#2091);
#1542=LINE('',#9388,#2092);
#1543=LINE('',#9390,#2093);
#1544=LINE('',#9393,#2094);
#1545=LINE('',#9394,#2095);
#1546=LINE('',#9397,#2096);
#1547=LINE('',#9401,#2097);
#1548=LINE('',#9404,#2098);
#1549=LINE('',#9407,#2099);
#1550=LINE('',#9409,#2100);
#1551=LINE('',#9411,#2101);
#1552=LINE('',#9413,#2102);
#1553=LINE('',#9415,#2103);
#1554=LINE('',#9417,#2104);
#1555=LINE('',#9419,#2105);
#1556=LINE('',#9421,#2106);
#1557=LINE('',#9423,#2107);
#1558=LINE('',#9424,#2108);
#1559=LINE('',#9428,#2109);
#1560=LINE('',#9432,#2110);
#1561=LINE('',#9436,#2111);
#1562=LINE('',#9438,#2112);
#1563=LINE('',#9440,#2113);
#1564=LINE('',#9442,#2114);
#1565=LINE('',#9444,#2115);
#1566=LINE('',#9446,#2116);
#1567=LINE('',#9448,#2117);
#1568=LINE('',#9450,#2118);
#1569=LINE('',#9451,#2119);
#1570=LINE('',#9454,#2120);
#1571=LINE('',#9459,#2121);
#1572=LINE('',#9462,#2122);
#1573=LINE('',#9463,#2123);
#1574=LINE('',#9469,#2124);
#1575=LINE('',#9474,#2125);
#1576=LINE('',#9478,#2126);
#1577=LINE('',#9482,#2127);
#1578=LINE('',#9486,#2128);
#1579=LINE('',#9489,#2129);
#1580=LINE('',#9491,#2130);
#1581=LINE('',#9494,#2131);
#1582=LINE('',#9496,#2132);
#1583=LINE('',#9497,#2133);
#1584=LINE('',#9500,#2134);
#1585=LINE('',#9501,#2135);
#1586=LINE('',#9504,#2136);
#1587=LINE('',#9505,#2137);
#1588=LINE('',#9508,#2138);
#1589=LINE('',#9509,#2139);
#1590=LINE('',#9521,#2140);
#1591=LINE('',#9525,#2141);
#1592=LINE('',#9528,#2142);
#1593=LINE('',#9530,#2143);
#1594=LINE('',#9532,#2144);
#1595=LINE('',#9533,#2145);
#1596=LINE('',#9542,#2146);
#1597=LINE('',#9548,#2147);
#1598=LINE('',#9554,#2148);
#1599=LINE('',#9560,#2149);
#1600=LINE('',#9565,#2150);
#1601=LINE('',#9569,#2151);
#1602=LINE('',#9574,#2152);
#1603=LINE('',#9578,#2153);
#1604=LINE('',#9582,#2154);
#1605=LINE('',#9585,#2155);
#1606=LINE('',#9589,#2156);
#1607=LINE('',#9593,#2157);
#1608=LINE('',#9597,#2158);
#1609=LINE('',#9600,#2159);
#1610=LINE('',#9602,#2160);
#1611=LINE('',#9603,#2161);
#1612=LINE('',#9606,#2162);
#1613=LINE('',#9608,#2163);
#1614=LINE('',#9612,#2164);
#1615=LINE('',#9614,#2165);
#1616=LINE('',#9617,#2166);
#1617=LINE('',#9618,#2167);
#1618=LINE('',#9621,#2168);
#1619=LINE('',#9623,#2169);
#1620=LINE('',#9627,#2170);
#1621=LINE('',#9629,#2171);
#1622=LINE('',#9632,#2172);
#1623=LINE('',#9633,#2173);
#1624=LINE('',#9636,#2174);
#1625=LINE('',#9638,#2175);
#1626=LINE('',#9639,#2176);
#1627=LINE('',#9642,#2177);
#1628=LINE('',#9643,#2178);
#1629=LINE('',#9646,#2179);
#1630=LINE('',#9647,#2180);
#1631=LINE('',#9650,#2181);
#1632=LINE('',#9651,#2182);
#1633=LINE('',#9654,#2183);
#1634=LINE('',#9655,#2184);
#1635=LINE('',#9658,#2185);
#1636=LINE('',#9659,#2186);
#1637=LINE('',#9664,#2187);
#1638=LINE('',#9668,#2188);
#1639=LINE('',#9672,#2189);
#1640=LINE('',#9675,#2190);
#1641=LINE('',#9678,#2191);
#1642=LINE('',#9681,#2192);
#1643=LINE('',#9684,#2193);
#1644=LINE('',#9687,#2194);
#1645=LINE('',#9690,#2195);
#1646=LINE('',#9692,#2196);
#1647=LINE('',#9695,#2197);
#1648=LINE('',#9699,#2198);
#1649=LINE('',#9703,#2199);
#1650=LINE('',#9707,#2200);
#1651=LINE('',#9711,#2201);
#1652=LINE('',#9715,#2202);
#1653=LINE('',#9718,#2203);
#1654=LINE('',#9719,#2204);
#1655=LINE('',#9721,#2205);
#1656=LINE('',#9723,#2206);
#1657=LINE('',#9726,#2207);
#1658=LINE('',#9728,#2208);
#1659=LINE('',#9730,#2209);
#1660=LINE('',#9737,#2210);
#1661=LINE('',#9743,#2211);
#1662=LINE('',#9749,#2212);
#1663=LINE('',#9755,#2213);
#1664=LINE('',#9760,#2214);
#1665=LINE('',#9764,#2215);
#1666=LINE('',#9769,#2216);
#1667=LINE('',#9773,#2217);
#1668=LINE('',#9777,#2218);
#1669=LINE('',#9780,#2219);
#1670=LINE('',#9784,#2220);
#1671=LINE('',#9788,#2221);
#1672=LINE('',#9792,#2222);
#1673=LINE('',#9795,#2223);
#1674=LINE('',#9797,#2224);
#1675=LINE('',#9798,#2225);
#1676=LINE('',#9801,#2226);
#1677=LINE('',#9803,#2227);
#1678=LINE('',#9807,#2228);
#1679=LINE('',#9809,#2229);
#1680=LINE('',#9812,#2230);
#1681=LINE('',#9813,#2231);
#1682=LINE('',#9816,#2232);
#1683=LINE('',#9818,#2233);
#1684=LINE('',#9822,#2234);
#1685=LINE('',#9824,#2235);
#1686=LINE('',#9827,#2236);
#1687=LINE('',#9828,#2237);
#1688=LINE('',#9831,#2238);
#1689=LINE('',#9833,#2239);
#1690=LINE('',#9834,#2240);
#1691=LINE('',#9837,#2241);
#1692=LINE('',#9838,#2242);
#1693=LINE('',#9841,#2243);
#1694=LINE('',#9842,#2244);
#1695=LINE('',#9845,#2245);
#1696=LINE('',#9846,#2246);
#1697=LINE('',#9849,#2247);
#1698=LINE('',#9850,#2248);
#1699=LINE('',#9853,#2249);
#1700=LINE('',#9854,#2250);
#1701=LINE('',#9859,#2251);
#1702=LINE('',#9863,#2252);
#1703=LINE('',#9867,#2253);
#1704=LINE('',#9870,#2254);
#1705=LINE('',#9873,#2255);
#1706=LINE('',#9876,#2256);
#1707=LINE('',#9879,#2257);
#1708=LINE('',#9882,#2258);
#1709=LINE('',#9885,#2259);
#1710=LINE('',#9887,#2260);
#1711=LINE('',#9890,#2261);
#1712=LINE('',#9894,#2262);
#1713=LINE('',#9898,#2263);
#1714=LINE('',#9902,#2264);
#1715=LINE('',#9906,#2265);
#1716=LINE('',#9910,#2266);
#1717=LINE('',#9913,#2267);
#1718=LINE('',#9914,#2268);
#1719=LINE('',#9916,#2269);
#1720=LINE('',#9918,#2270);
#1721=LINE('',#9921,#2271);
#1722=LINE('',#9923,#2272);
#1723=LINE('',#9925,#2273);
#1724=LINE('',#9931,#2274);
#1725=LINE('',#9935,#2275);
#1726=LINE('',#9940,#2276);
#1727=LINE('',#9944,#2277);
#1728=LINE('',#9948,#2278);
#1729=LINE('',#9951,#2279);
#1730=LINE('',#9954,#2280);
#1731=LINE('',#9957,#2281);
#1732=LINE('',#9960,#2282);
#1733=LINE('',#9963,#2283);
#1734=LINE('',#9966,#2284);
#1735=LINE('',#9969,#2285);
#1736=LINE('',#9972,#2286);
#1737=LINE('',#9974,#2287);
#1738=LINE('',#9978,#2288);
#1739=LINE('',#9980,#2289);
#1740=LINE('',#9984,#2290);
#1741=LINE('',#9986,#2291);
#1742=LINE('',#9990,#2292);
#1743=LINE('',#9992,#2293);
#1744=LINE('',#9995,#2294);
#1745=LINE('',#9996,#2295);
#1746=LINE('',#9998,#2296);
#1747=LINE('',#9999,#2297);
#1748=LINE('',#10002,#2298);
#1749=LINE('',#10004,#2299);
#1750=LINE('',#10005,#2300);
#1751=LINE('',#10008,#2301);
#1752=LINE('',#10009,#2302);
#1753=LINE('',#10012,#2303);
#1754=LINE('',#10013,#2304);
#1755=LINE('',#10016,#2305);
#1756=LINE('',#10017,#2306);
#1757=LINE('',#10020,#2307);
#1758=LINE('',#10021,#2308);
#1759=LINE('',#10024,#2309);
#1760=LINE('',#10025,#2310);
#1761=LINE('',#10030,#2311);
#1762=LINE('',#10035,#2312);
#1763=LINE('',#10039,#2313);
#1764=LINE('',#10043,#2314);
#1765=LINE('',#10047,#2315);
#1766=LINE('',#10050,#2316);
#1767=LINE('',#10053,#2317);
#1768=LINE('',#10055,#2318);
#1769=LINE('',#10059,#2319);
#1770=LINE('',#10061,#2320);
#1771=LINE('',#10065,#2321);
#1772=LINE('',#10067,#2322);
#1773=LINE('',#10071,#2323);
#1774=LINE('',#10073,#2324);
#1775=LINE('',#10076,#2325);
#1776=LINE('',#10078,#2326);
#1777=LINE('',#10082,#2327);
#1778=LINE('',#10085,#2328);
#1779=LINE('',#10087,#2329);
#1780=LINE('',#10088,#2330);
#1781=LINE('',#10090,#2331);
#1782=LINE('',#10094,#2332);
#1783=LINE('',#10095,#2333);
#1784=VECTOR('',#6630,10.);
#1785=VECTOR('',#6637,10.);
#1786=VECTOR('',#6644,10.);
#1787=VECTOR('',#6651,10.);
#1788=VECTOR('',#6658,10.);
#1789=VECTOR('',#6665,10.);
#1790=VECTOR('',#6672,10.);
#1791=VECTOR('',#6679,10.);
#1792=VECTOR('',#6686,10.);
#1793=VECTOR('',#6689,10.);
#1794=VECTOR('',#6692,10.);
#1795=VECTOR('',#6693,10.);
#1796=VECTOR('',#6694,10.);
#1797=VECTOR('',#6697,10.);
#1798=VECTOR('',#6700,10.);
#1799=VECTOR('',#6703,10.);
#1800=VECTOR('',#6710,10.);
#1801=VECTOR('',#6711,10.);
#1802=VECTOR('',#6714,10.);
#1803=VECTOR('',#6715,10.);
#1804=VECTOR('',#6720,10.);
#1805=VECTOR('',#6725,10.);
#1806=VECTOR('',#6728,10.);
#1807=VECTOR('',#6731,10.);
#1808=VECTOR('',#6740,3.);
#1809=VECTOR('',#6745,10.);
#1810=VECTOR('',#6746,10.);
#1811=VECTOR('',#6747,10.);
#1812=VECTOR('',#6748,10.);
#1813=VECTOR('',#6751,10.);
#1814=VECTOR('',#6752,10.);
#1815=VECTOR('',#6753,10.);
#1816=VECTOR('',#6756,10.);
#1817=VECTOR('',#6757,10.);
#1818=VECTOR('',#6758,10.);
#1819=VECTOR('',#6761,10.);
#1820=VECTOR('',#6762,10.);
#1821=VECTOR('',#6763,10.);
#1822=VECTOR('',#6766,10.);
#1823=VECTOR('',#6767,10.);
#1824=VECTOR('',#6768,10.);
#1825=VECTOR('',#6771,10.);
#1826=VECTOR('',#6772,10.);
#1827=VECTOR('',#6773,10.);
#1828=VECTOR('',#6776,10.);
#1829=VECTOR('',#6777,10.);
#1830=VECTOR('',#6778,10.);
#1831=VECTOR('',#6781,10.);
#1832=VECTOR('',#6782,10.);
#1833=VECTOR('',#6783,10.);
#1834=VECTOR('',#6786,10.);
#1835=VECTOR('',#6787,10.);
#1836=VECTOR('',#6788,10.);
#1837=VECTOR('',#6791,10.);
#1838=VECTOR('',#6792,10.);
#1839=VECTOR('',#6793,10.);
#1840=VECTOR('',#6796,10.);
#1841=VECTOR('',#6797,10.);
#1842=VECTOR('',#6798,10.);
#1843=VECTOR('',#6801,10.);
#1844=VECTOR('',#6802,10.);
#1845=VECTOR('',#6805,10.);
#1846=VECTOR('',#6806,10.);
#1847=VECTOR('',#6807,10.);
#1848=VECTOR('',#6810,10.);
#1849=VECTOR('',#6811,10.);
#1850=VECTOR('',#6814,10.);
#1851=VECTOR('',#6815,10.);
#1852=VECTOR('',#6818,10.);
#1853=VECTOR('',#6819,10.);
#1854=VECTOR('',#6822,10.);
#1855=VECTOR('',#6823,10.);
#1856=VECTOR('',#6826,10.);
#1857=VECTOR('',#6827,10.);
#1858=VECTOR('',#6832,10.);
#1859=VECTOR('',#6833,10.);
#1860=VECTOR('',#6834,10.);
#1861=VECTOR('',#6837,10.);
#1862=VECTOR('',#6838,10.);
#1863=VECTOR('',#6841,10.);
#1864=VECTOR('',#6842,10.);
#1865=VECTOR('',#6843,10.);
#1866=VECTOR('',#6844,10.);
#1867=VECTOR('',#6847,10.);
#1868=VECTOR('',#6850,10.);
#1869=VECTOR('',#6869,10.);
#1870=VECTOR('',#6870,10.);
#1871=VECTOR('',#6879,10.);
#1872=VECTOR('',#6880,10.);
#1873=VECTOR('',#6881,10.);
#1874=VECTOR('',#6894,10.);
#1875=VECTOR('',#6895,10.);
#1876=VECTOR('',#6904,10.);
#1877=VECTOR('',#6905,10.);
#1878=VECTOR('',#6906,10.);
#1879=VECTOR('',#6911,3.);
#1880=VECTOR('',#6918,3.);
#1881=VECTOR('',#6925,3.);
#1882=VECTOR('',#6932,3.);
#1883=VECTOR('',#6937,10.);
#1884=VECTOR('',#6938,10.);
#1885=VECTOR('',#6941,10.);
#1886=VECTOR('',#6944,10.);
#1887=VECTOR('',#6947,10.);
#1888=VECTOR('',#6950,10.);
#1889=VECTOR('',#6953,10.);
#1890=VECTOR('',#6954,10.);
#1891=VECTOR('',#6955,10.);
#1892=VECTOR('',#6956,10.);
#1893=VECTOR('',#6959,10.);
#1894=VECTOR('',#6960,10.);
#1895=VECTOR('',#6961,10.);
#1896=VECTOR('',#6962,10.);
#1897=VECTOR('',#6963,10.);
#1898=VECTOR('',#6964,10.);
#1899=VECTOR('',#6965,10.);
#1900=VECTOR('',#6966,10.);
#1901=VECTOR('',#6971,10.);
#1902=VECTOR('',#6974,10.);
#1903=VECTOR('',#6979,10.);
#1904=VECTOR('',#6982,10.);
#1905=VECTOR('',#6987,10.);
#1906=VECTOR('',#6990,10.);
#1907=VECTOR('',#6995,10.);
#1908=VECTOR('',#6998,10.);
#1909=VECTOR('',#7001,10.);
#1910=VECTOR('',#7004,10.);
#1911=VECTOR('',#7009,10.);
#1912=VECTOR('',#7012,10.);
#1913=VECTOR('',#7015,10.);
#1914=VECTOR('',#7016,10.);
#1915=VECTOR('',#7019,10.);
#1916=VECTOR('',#7020,10.);
#1917=VECTOR('',#7025,10.);
#1918=VECTOR('',#7026,10.);
#1919=VECTOR('',#7031,10.);
#1920=VECTOR('',#7032,10.);
#1921=VECTOR('',#7035,10.);
#1922=VECTOR('',#7036,10.);
#1923=VECTOR('',#7041,10.);
#1924=VECTOR('',#7042,10.);
#1925=VECTOR('',#7047,10.);
#1926=VECTOR('',#7048,10.);
#1927=VECTOR('',#7051,10.);
#1928=VECTOR('',#7052,10.);
#1929=VECTOR('',#7053,10.);
#1930=VECTOR('',#7056,10.);
#1931=VECTOR('',#7057,10.);
#1932=VECTOR('',#7060,10.);
#1933=VECTOR('',#7061,10.);
#1934=VECTOR('',#7064,10.);
#1935=VECTOR('',#7065,10.);
#1936=VECTOR('',#7068,10.);
#1937=VECTOR('',#7069,10.);
#1938=VECTOR('',#7072,10.);
#1939=VECTOR('',#7073,10.);
#1940=VECTOR('',#7080,10.);
#1941=VECTOR('',#7085,10.);
#1942=VECTOR('',#7088,10.);
#1943=VECTOR('',#7093,10.);
#1944=VECTOR('',#7118,10.);
#1945=VECTOR('',#7121,10.);
#1946=VECTOR('',#7124,10.);
#1947=VECTOR('',#7127,10.);
#1948=VECTOR('',#7130,10.);
#1949=VECTOR('',#7137,10.);
#1950=VECTOR('',#7140,10.);
#1951=VECTOR('',#7145,10.);
#1952=VECTOR('',#7148,10.);
#1953=VECTOR('',#7153,10.);
#1954=VECTOR('',#7156,10.);
#1955=VECTOR('',#7159,10.);
#1956=VECTOR('',#7162,10.);
#1957=VECTOR('',#7165,10.);
#1958=VECTOR('',#7168,10.);
#1959=VECTOR('',#7171,10.);
#1960=VECTOR('',#7174,10.);
#1961=VECTOR('',#7177,10.);
#1962=VECTOR('',#7178,10.);
#1963=VECTOR('',#7183,10.);
#1964=VECTOR('',#7184,10.);
#1965=VECTOR('',#7189,10.);
#1966=VECTOR('',#7190,10.);
#1967=VECTOR('',#7195,10.);
#1968=VECTOR('',#7196,10.);
#1969=VECTOR('',#7201,10.);
#1970=VECTOR('',#7202,10.);
#1971=VECTOR('',#7205,10.);
#1972=VECTOR('',#7206,10.);
#1973=VECTOR('',#7209,10.);
#1974=VECTOR('',#7210,10.);
#1975=VECTOR('',#7211,10.);
#1976=VECTOR('',#7214,10.);
#1977=VECTOR('',#7215,10.);
#1978=VECTOR('',#7218,10.);
#1979=VECTOR('',#7219,10.);
#1980=VECTOR('',#7222,10.);
#1981=VECTOR('',#7223,10.);
#1982=VECTOR('',#7226,10.);
#1983=VECTOR('',#7227,10.);
#1984=VECTOR('',#7230,10.);
#1985=VECTOR('',#7231,10.);
#1986=VECTOR('',#7236,10.);
#1987=VECTOR('',#7243,10.);
#1988=VECTOR('',#7248,10.);
#1989=VECTOR('',#7253,10.);
#1990=VECTOR('',#7258,10.);
#1991=VECTOR('',#7261,10.);
#1992=VECTOR('',#7264,10.);
#1993=VECTOR('',#7265,10.);
#1994=VECTOR('',#7270,10.);
#1995=VECTOR('',#7271,10.);
#1996=VECTOR('',#7276,10.);
#1997=VECTOR('',#7277,10.);
#1998=VECTOR('',#7282,10.);
#1999=VECTOR('',#7283,10.);
#2000=VECTOR('',#7288,10.);
#2001=VECTOR('',#7289,10.);
#2002=VECTOR('',#7294,10.);
#2003=VECTOR('',#7299,10.);
#2004=VECTOR('',#7302,10.);
#2005=VECTOR('',#7303,10.);
#2006=VECTOR('',#7306,10.);
#2007=VECTOR('',#7313,10.);
#2008=VECTOR('',#7314,10.);
#2009=VECTOR('',#7325,3.00000000000001);
#2010=VECTOR('',#7332,3.);
#2011=VECTOR('',#7339,2.99999999999999);
#2012=VECTOR('',#7346,3.);
#2013=VECTOR('',#7353,3.);
#2014=VECTOR('',#7360,2.99999999999999);
#2015=VECTOR('',#7367,2.99999999999999);
#2016=VECTOR('',#7374,3.);
#2017=VECTOR('',#7381,3.);
#2018=VECTOR('',#7388,2.99999999999999);
#2019=VECTOR('',#7393,10.);
#2020=VECTOR('',#7396,10.);
#2021=VECTOR('',#7401,10.);
#2022=VECTOR('',#7404,10.);
#2023=VECTOR('',#7407,10.);
#2024=VECTOR('',#7410,10.);
#2025=VECTOR('',#7413,10.);
#2026=VECTOR('',#7416,10.);
#2027=VECTOR('',#7419,10.);
#2028=VECTOR('',#7420,10.);
#2029=VECTOR('',#7425,10.);
#2030=VECTOR('',#7426,10.);
#2031=VECTOR('',#7431,10.);
#2032=VECTOR('',#7432,10.);
#2033=VECTOR('',#7437,10.);
#2034=VECTOR('',#7438,10.);
#2035=VECTOR('',#7441,10.);
#2036=VECTOR('',#7442,10.);
#2037=VECTOR('',#7443,10.);
#2038=VECTOR('',#7446,10.);
#2039=VECTOR('',#7447,10.);
#2040=VECTOR('',#7450,10.);
#2041=VECTOR('',#7451,10.);
#2042=VECTOR('',#7454,10.);
#2043=VECTOR('',#7455,10.);
#2044=VECTOR('',#7460,10.);
#2045=VECTOR('',#7467,10.);
#2046=VECTOR('',#7472,10.);
#2047=VECTOR('',#7477,10.);
#2048=VECTOR('',#7482,10.);
#2049=VECTOR('',#7483,10.);
#2050=VECTOR('',#7488,10.);
#2051=VECTOR('',#7489,10.);
#2052=VECTOR('',#7494,10.);
#2053=VECTOR('',#7495,10.);
#2054=VECTOR('',#7500,10.);
#2055=VECTOR('',#7501,10.);
#2056=VECTOR('',#7504,10.);
#2057=VECTOR('',#7505,10.);
#2058=VECTOR('',#7508,10.);
#2059=VECTOR('',#7521,3.00000000000001);
#2060=VECTOR('',#7528,3.);
#2061=VECTOR('',#7533,10.);
#2062=VECTOR('',#7534,10.);
#2063=VECTOR('',#7535,10.);
#2064=VECTOR('',#7536,10.);
#2065=VECTOR('',#7537,10.);
#2066=VECTOR('',#7538,10.);
#2067=VECTOR('',#7539,10.);
#2068=VECTOR('',#7540,10.);
#2069=VECTOR('',#7543,10.);
#2070=VECTOR('',#7544,10.);
#2071=VECTOR('',#7545,10.);
#2072=VECTOR('',#7548,10.);
#2073=VECTOR('',#7549,10.);
#2074=VECTOR('',#7552,10.);
#2075=VECTOR('',#7553,10.);
#2076=VECTOR('',#7556,10.);
#2077=VECTOR('',#7557,10.);
#2078=VECTOR('',#7560,10.);
#2079=VECTOR('',#7561,10.);
#2080=VECTOR('',#7564,10.);
#2081=VECTOR('',#7565,10.);
#2082=VECTOR('',#7568,10.);
#2083=VECTOR('',#7569,10.);
#2084=VECTOR('',#7572,10.);
#2085=VECTOR('',#7581,3.);
#2086=VECTOR('',#7590,3.);
#2087=VECTOR('',#7599,3.);
#2088=VECTOR('',#7606,10.);
#2089=VECTOR('',#7609,10.);
#2090=VECTOR('',#7614,10.);
#2091=VECTOR('',#7615,10.);
#2092=VECTOR('',#7620,10.);
#2093=VECTOR('',#7621,10.);
#2094=VECTOR('',#7626,10.);
#2095=VECTOR('',#7627,10.);
#2096=VECTOR('',#7630,10.);
#2097=VECTOR('',#7633,10.);
#2098=VECTOR('',#7636,10.);
#2099=VECTOR('',#7639,10.);
#2100=VECTOR('',#7640,10.);
#2101=VECTOR('',#7641,10.);
#2102=VECTOR('',#7642,10.);
#2103=VECTOR('',#7643,10.);
#2104=VECTOR('',#7644,10.);
#2105=VECTOR('',#7645,10.);
#2106=VECTOR('',#7646,10.);
#2107=VECTOR('',#7647,10.);
#2108=VECTOR('',#7648,10.);
#2109=VECTOR('',#7653,10.);
#2110=VECTOR('',#7656,10.);
#2111=VECTOR('',#7661,10.);
#2112=VECTOR('',#7662,10.);
#2113=VECTOR('',#7663,10.);
#2114=VECTOR('',#7664,10.);
#2115=VECTOR('',#7665,10.);
#2116=VECTOR('',#7666,10.);
#2117=VECTOR('',#7667,10.);
#2118=VECTOR('',#7668,10.);
#2119=VECTOR('',#7669,10.);
#2120=VECTOR('',#7672,10.);
#2121=VECTOR('',#7679,10.);
#2122=VECTOR('',#7682,10.);
#2123=VECTOR('',#7683,10.);
#2124=VECTOR('',#7690,10.);
#2125=VECTOR('',#7697,10.);
#2126=VECTOR('',#7702,10.);
#2127=VECTOR('',#7707,10.);
#2128=VECTOR('',#7712,10.);
#2129=VECTOR('',#7717,10.);
#2130=VECTOR('',#7720,10.);
#2131=VECTOR('',#7723,10.);
#2132=VECTOR('',#7724,10.);
#2133=VECTOR('',#7725,10.);
#2134=VECTOR('',#7728,10.);
#2135=VECTOR('',#7729,10.);
#2136=VECTOR('',#7732,10.);
#2137=VECTOR('',#7733,10.);
#2138=VECTOR('',#7736,10.);
#2139=VECTOR('',#7737,10.);
#2140=VECTOR('',#7758,10.);
#2141=VECTOR('',#7763,10.);
#2142=VECTOR('',#7768,10.);
#2143=VECTOR('',#7771,10.);
#2144=VECTOR('',#7774,10.);
#2145=VECTOR('',#7775,10.);
#2146=VECTOR('',#7788,3.);
#2147=VECTOR('',#7795,3.);
#2148=VECTOR('',#7802,3.);
#2149=VECTOR('',#7809,3.);
#2150=VECTOR('',#7814,10.);
#2151=VECTOR('',#7817,10.);
#2152=VECTOR('',#7822,10.);
#2153=VECTOR('',#7825,10.);
#2154=VECTOR('',#7830,10.);
#2155=VECTOR('',#7833,10.);
#2156=VECTOR('',#7836,10.);
#2157=VECTOR('',#7839,10.);
#2158=VECTOR('',#7844,10.);
#2159=VECTOR('',#7847,10.);
#2160=VECTOR('',#7850,10.);
#2161=VECTOR('',#7851,10.);
#2162=VECTOR('',#7854,10.);
#2163=VECTOR('',#7855,10.);
#2164=VECTOR('',#7860,10.);
#2165=VECTOR('',#7861,10.);
#2166=VECTOR('',#7866,10.);
#2167=VECTOR('',#7867,10.);
#2168=VECTOR('',#7870,10.);
#2169=VECTOR('',#7871,10.);
#2170=VECTOR('',#7876,10.);
#2171=VECTOR('',#7877,10.);
#2172=VECTOR('',#7882,10.);
#2173=VECTOR('',#7883,10.);
#2174=VECTOR('',#7886,10.);
#2175=VECTOR('',#7887,10.);
#2176=VECTOR('',#7888,10.);
#2177=VECTOR('',#7891,10.);
#2178=VECTOR('',#7892,10.);
#2179=VECTOR('',#7895,10.);
#2180=VECTOR('',#7896,10.);
#2181=VECTOR('',#7899,10.);
#2182=VECTOR('',#7900,10.);
#2183=VECTOR('',#7903,10.);
#2184=VECTOR('',#7904,10.);
#2185=VECTOR('',#7907,10.);
#2186=VECTOR('',#7908,10.);
#2187=VECTOR('',#7913,10.);
#2188=VECTOR('',#7916,10.);
#2189=VECTOR('',#7921,10.);
#2190=VECTOR('',#7924,10.);
#2191=VECTOR('',#7927,10.);
#2192=VECTOR('',#7930,10.);
#2193=VECTOR('',#7933,10.);
#2194=VECTOR('',#7936,10.);
#2195=VECTOR('',#7939,10.);
#2196=VECTOR('',#7942,10.);
#2197=VECTOR('',#7945,10.);
#2198=VECTOR('',#7950,10.);
#2199=VECTOR('',#7955,10.);
#2200=VECTOR('',#7960,10.);
#2201=VECTOR('',#7965,10.);
#2202=VECTOR('',#7970,10.);
#2203=VECTOR('',#7975,10.);
#2204=VECTOR('',#7976,10.);
#2205=VECTOR('',#7979,10.);
#2206=VECTOR('',#7982,10.);
#2207=VECTOR('',#7987,10.);
#2208=VECTOR('',#7990,10.);
#2209=VECTOR('',#7993,10.);
#2210=VECTOR('',#8002,3.);
#2211=VECTOR('',#8009,3.);
#2212=VECTOR('',#8016,3.);
#2213=VECTOR('',#8023,3.);
#2214=VECTOR('',#8028,10.);
#2215=VECTOR('',#8031,10.);
#2216=VECTOR('',#8036,10.);
#2217=VECTOR('',#8039,10.);
#2218=VECTOR('',#8044,10.);
#2219=VECTOR('',#8047,10.);
#2220=VECTOR('',#8050,10.);
#2221=VECTOR('',#8053,10.);
#2222=VECTOR('',#8058,10.);
#2223=VECTOR('',#8061,10.);
#2224=VECTOR('',#8064,10.);
#2225=VECTOR('',#8065,10.);
#2226=VECTOR('',#8068,10.);
#2227=VECTOR('',#8069,10.);
#2228=VECTOR('',#8074,10.);
#2229=VECTOR('',#8075,10.);
#2230=VECTOR('',#8080,10.);
#2231=VECTOR('',#8081,10.);
#2232=VECTOR('',#8084,10.);
#2233=VECTOR('',#8085,10.);
#2234=VECTOR('',#8090,10.);
#2235=VECTOR('',#8091,10.);
#2236=VECTOR('',#8096,10.);
#2237=VECTOR('',#8097,10.);
#2238=VECTOR('',#8100,10.);
#2239=VECTOR('',#8101,10.);
#2240=VECTOR('',#8102,10.);
#2241=VECTOR('',#8105,10.);
#2242=VECTOR('',#8106,10.);
#2243=VECTOR('',#8109,10.);
#2244=VECTOR('',#8110,10.);
#2245=VECTOR('',#8113,10.);
#2246=VECTOR('',#8114,10.);
#2247=VECTOR('',#8117,10.);
#2248=VECTOR('',#8118,10.);
#2249=VECTOR('',#8121,10.);
#2250=VECTOR('',#8122,10.);
#2251=VECTOR('',#8127,10.);
#2252=VECTOR('',#8130,10.);
#2253=VECTOR('',#8135,10.);
#2254=VECTOR('',#8138,10.);
#2255=VECTOR('',#8141,10.);
#2256=VECTOR('',#8144,10.);
#2257=VECTOR('',#8147,10.);
#2258=VECTOR('',#8150,10.);
#2259=VECTOR('',#8153,10.);
#2260=VECTOR('',#8156,10.);
#2261=VECTOR('',#8159,10.);
#2262=VECTOR('',#8164,10.);
#2263=VECTOR('',#8169,10.);
#2264=VECTOR('',#8174,10.);
#2265=VECTOR('',#8179,10.);
#2266=VECTOR('',#8184,10.);
#2267=VECTOR('',#8189,10.);
#2268=VECTOR('',#8190,10.);
#2269=VECTOR('',#8193,10.);
#2270=VECTOR('',#8196,10.);
#2271=VECTOR('',#8201,10.);
#2272=VECTOR('',#8204,10.);
#2273=VECTOR('',#8207,10.);
#2274=VECTOR('',#8214,10.);
#2275=VECTOR('',#8217,10.);
#2276=VECTOR('',#8222,10.);
#2277=VECTOR('',#8225,10.);
#2278=VECTOR('',#8230,10.);
#2279=VECTOR('',#8233,10.);
#2280=VECTOR('',#8236,10.);
#2281=VECTOR('',#8239,10.);
#2282=VECTOR('',#8242,10.);
#2283=VECTOR('',#8245,10.);
#2284=VECTOR('',#8248,10.);
#2285=VECTOR('',#8251,10.);
#2286=VECTOR('',#8254,10.);
#2287=VECTOR('',#8255,10.);
#2288=VECTOR('',#8260,10.);
#2289=VECTOR('',#8261,10.);
#2290=VECTOR('',#8266,10.);
#2291=VECTOR('',#8267,10.);
#2292=VECTOR('',#8272,10.);
#2293=VECTOR('',#8273,10.);
#2294=VECTOR('',#8278,10.);
#2295=VECTOR('',#8279,10.);
#2296=VECTOR('',#8282,10.);
#2297=VECTOR('',#8283,10.);
#2298=VECTOR('',#8286,10.);
#2299=VECTOR('',#8287,10.);
#2300=VECTOR('',#8288,10.);
#2301=VECTOR('',#8291,10.);
#2302=VECTOR('',#8292,10.);
#2303=VECTOR('',#8295,10.);
#2304=VECTOR('',#8296,10.);
#2305=VECTOR('',#8299,10.);
#2306=VECTOR('',#8300,10.);
#2307=VECTOR('',#8303,10.);
#2308=VECTOR('',#8304,10.);
#2309=VECTOR('',#8307,10.);
#2310=VECTOR('',#8308,10.);
#2311=VECTOR('',#8313,10.);
#2312=VECTOR('',#8320,10.);
#2313=VECTOR('',#8325,10.);
#2314=VECTOR('',#8330,10.);
#2315=VECTOR('',#8335,10.);
#2316=VECTOR('',#8338,10.);
#2317=VECTOR('',#8341,10.);
#2318=VECTOR('',#8342,10.);
#2319=VECTOR('',#8347,10.);
#2320=VECTOR('',#8348,10.);
#2321=VECTOR('',#8353,10.);
#2322=VECTOR('',#8354,10.);
#2323=VECTOR('',#8359,10.);
#2324=VECTOR('',#8360,10.);
#2325=VECTOR('',#8365,10.);
#2326=VECTOR('',#8366,10.);
#2327=VECTOR('',#8371,10.);
#2328=VECTOR('',#8376,10.);
#2329=VECTOR('',#8379,10.);
#2330=VECTOR('',#8380,10.);
#2331=VECTOR('',#8383,10.);
#2332=VECTOR('',#8390,10.);
#2333=VECTOR('',#8391,10.);
#2334=CIRCLE('',#6003,10.);
#2335=CIRCLE('',#6004,10.);
#2336=CIRCLE('',#6006,10.);
#2337=CIRCLE('',#6007,10.);
#2338=CIRCLE('',#6009,10.);
#2339=CIRCLE('',#6010,10.);
#2340=CIRCLE('',#6012,10.);
#2341=CIRCLE('',#6013,10.);
#2342=CIRCLE('',#6015,10.);
#2343=CIRCLE('',#6016,10.);
#2344=CIRCLE('',#6018,10.);
#2345=CIRCLE('',#6019,10.);
#2346=CIRCLE('',#6021,10.);
#2347=CIRCLE('',#6022,10.);
#2348=CIRCLE('',#6024,10.);
#2349=CIRCLE('',#6025,10.);
#2350=CIRCLE('',#6027,10.);
#2351=CIRCLE('',#6028,10.);
#2352=CIRCLE('',#6031,10.);
#2353=CIRCLE('',#6032,10.);
#2354=CIRCLE('',#6033,10.);
#2355=CIRCLE('',#6035,10.);
#2356=CIRCLE('',#6038,10.);
#2357=CIRCLE('',#6040,10.);
#2358=CIRCLE('',#6046,3.);
#2359=CIRCLE('',#6047,3.);
#2360=CIRCLE('',#6076,4.);
#2361=CIRCLE('',#6077,1.);
#2362=CIRCLE('',#6078,5.);
#2363=CIRCLE('',#6080,4.);
#2364=CIRCLE('',#6082,1.);
#2365=CIRCLE('',#6083,5.);
#2366=CIRCLE('',#6086,4.);
#2367=CIRCLE('',#6087,1.);
#2368=CIRCLE('',#6088,5.);
#2369=CIRCLE('',#6090,4.);
#2370=CIRCLE('',#6092,1.);
#2371=CIRCLE('',#6093,5.);
#2372=CIRCLE('',#6096,3.);
#2373=CIRCLE('',#6097,3.);
#2374=CIRCLE('',#6099,3.);
#2375=CIRCLE('',#6100,3.);
#2376=CIRCLE('',#6102,3.);
#2377=CIRCLE('',#6103,3.);
#2378=CIRCLE('',#6105,3.);
#2379=CIRCLE('',#6106,3.);
#2380=CIRCLE('',#6238,3.00000000000001);
#2381=CIRCLE('',#6239,3.00000000000001);
#2382=CIRCLE('',#6241,3.);
#2383=CIRCLE('',#6242,3.);
#2384=CIRCLE('',#6244,2.99999999999999);
#2385=CIRCLE('',#6245,2.99999999999999);
#2386=CIRCLE('',#6247,3.);
#2387=CIRCLE('',#6248,3.);
#2388=CIRCLE('',#6250,3.);
#2389=CIRCLE('',#6251,3.);
#2390=CIRCLE('',#6253,2.99999999999999);
#2391=CIRCLE('',#6254,2.99999999999999);
#2392=CIRCLE('',#6256,2.99999999999999);
#2393=CIRCLE('',#6257,2.99999999999999);
#2394=CIRCLE('',#6259,3.);
#2395=CIRCLE('',#6260,3.);
#2396=CIRCLE('',#6262,3.);
#2397=CIRCLE('',#6263,3.);
#2398=CIRCLE('',#6265,2.99999999999999);
#2399=CIRCLE('',#6266,2.99999999999999);
#2400=CIRCLE('',#6311,3.00000000000001);
#2401=CIRCLE('',#6312,3.00000000000001);
#2402=CIRCLE('',#6314,3.);
#2403=CIRCLE('',#6315,3.);
#2404=CIRCLE('',#6328,3.);
#2405=CIRCLE('',#6329,3.);
#2406=CIRCLE('',#6332,3.);
#2407=CIRCLE('',#6333,3.);
#2408=CIRCLE('',#6336,3.);
#2409=CIRCLE('',#6337,3.);
#2410=CIRCLE('',#6348,1.);
#2411=CIRCLE('',#6349,1.);
#2412=CIRCLE('',#6353,1.);
#2413=CIRCLE('',#6354,1.);
#2414=CIRCLE('',#6401,3.);
#2415=CIRCLE('',#6402,3.);
#2416=CIRCLE('',#6404,3.);
#2417=CIRCLE('',#6405,3.);
#2418=CIRCLE('',#6407,3.);
#2419=CIRCLE('',#6408,3.);
#2420=CIRCLE('',#6410,3.);
#2421=CIRCLE('',#6411,3.);
#2422=CIRCLE('',#6476,3.);
#2423=CIRCLE('',#6477,3.);
#2424=CIRCLE('',#6479,3.);
#2425=CIRCLE('',#6480,3.);
#2426=CIRCLE('',#6482,3.);
#2427=CIRCLE('',#6483,3.);
#2428=CIRCLE('',#6485,3.);
#2429=CIRCLE('',#6486,3.);
#2430=VERTEX_POINT('',#8419);
#2431=VERTEX_POINT('',#8421);
#2432=VERTEX_POINT('',#8425);
#2433=VERTEX_POINT('',#8427);
#2434=VERTEX_POINT('',#8431);
#2435=VERTEX_POINT('',#8433);
#2436=VERTEX_POINT('',#8437);
#2437=VERTEX_POINT('',#8439);
#2438=VERTEX_POINT('',#8443);
#2439=VERTEX_POINT('',#8445);
#2440=VERTEX_POINT('',#8449);
#2441=VERTEX_POINT('',#8451);
#2442=VERTEX_POINT('',#8455);
#2443=VERTEX_POINT('',#8457);
#2444=VERTEX_POINT('',#8461);
#2445=VERTEX_POINT('',#8463);
#2446=VERTEX_POINT('',#8467);
#2447=VERTEX_POINT('',#8468);
#2448=VERTEX_POINT('',#8470);
#2449=VERTEX_POINT('',#8472);
#2450=VERTEX_POINT('',#8476);
#2451=VERTEX_POINT('',#8478);
#2452=VERTEX_POINT('',#8482);
#2453=VERTEX_POINT('',#8484);
#2454=VERTEX_POINT('',#8486);
#2455=VERTEX_POINT('',#8488);
#2456=VERTEX_POINT('',#8490);
#2457=VERTEX_POINT('',#8494);
#2458=VERTEX_POINT('',#8495);
#2459=VERTEX_POINT('',#8500);
#2460=VERTEX_POINT('',#8504);
#2461=VERTEX_POINT('',#8508);
#2462=VERTEX_POINT('',#8518);
#2463=VERTEX_POINT('',#8520);
#2464=VERTEX_POINT('',#8524);
#2465=VERTEX_POINT('',#8525);
#2466=VERTEX_POINT('',#8527);
#2467=VERTEX_POINT('',#8529);
#2468=VERTEX_POINT('',#8533);
#2469=VERTEX_POINT('',#8535);
#2470=VERTEX_POINT('',#8539);
#2471=VERTEX_POINT('',#8541);
#2472=VERTEX_POINT('',#8545);
#2473=VERTEX_POINT('',#8547);
#2474=VERTEX_POINT('',#8551);
#2475=VERTEX_POINT('',#8553);
#2476=VERTEX_POINT('',#8557);
#2477=VERTEX_POINT('',#8559);
#2478=VERTEX_POINT('',#8563);
#2479=VERTEX_POINT('',#8565);
#2480=VERTEX_POINT('',#8569);
#2481=VERTEX_POINT('',#8571);
#2482=VERTEX_POINT('',#8575);
#2483=VERTEX_POINT('',#8577);
#2484=VERTEX_POINT('',#8581);
#2485=VERTEX_POINT('',#8583);
#2486=VERTEX_POINT('',#8587);
#2487=VERTEX_POINT('',#8589);
#2488=VERTEX_POINT('',#8596);
#2489=VERTEX_POINT('',#8598);
#2490=VERTEX_POINT('',#8602);
#2491=VERTEX_POINT('',#8606);
#2492=VERTEX_POINT('',#8610);
#2493=VERTEX_POINT('',#8614);
#2494=VERTEX_POINT('',#8618);
#2495=VERTEX_POINT('',#8623);
#2496=VERTEX_POINT('',#8625);
#2497=VERTEX_POINT('',#8629);
#2498=VERTEX_POINT('',#8634);
#2499=VERTEX_POINT('',#8636);
#2500=VERTEX_POINT('',#8647);
#2501=VERTEX_POINT('',#8648);
#2502=VERTEX_POINT('',#8650);
#2503=VERTEX_POINT('',#8652);
#2504=VERTEX_POINT('',#8665);
#2505=VERTEX_POINT('',#8666);
#2506=VERTEX_POINT('',#8671);
#2507=VERTEX_POINT('',#8672);
#2508=VERTEX_POINT('',#8686);
#2509=VERTEX_POINT('',#8688);
#2510=VERTEX_POINT('',#8692);
#2511=VERTEX_POINT('',#8693);
#2512=VERTEX_POINT('',#8695);
#2513=VERTEX_POINT('',#8697);
#2514=VERTEX_POINT('',#8710);
#2515=VERTEX_POINT('',#8711);
#2516=VERTEX_POINT('',#8716);
#2517=VERTEX_POINT('',#8717);
#2518=VERTEX_POINT('',#8731);
#2519=VERTEX_POINT('',#8733);
#2520=VERTEX_POINT('',#8737);
#2521=VERTEX_POINT('',#8739);
#2522=VERTEX_POINT('',#8743);
#2523=VERTEX_POINT('',#8745);
#2524=VERTEX_POINT('',#8749);
#2525=VERTEX_POINT('',#8751);
#2526=VERTEX_POINT('',#8755);
#2527=VERTEX_POINT('',#8757);
#2528=VERTEX_POINT('',#8764);
#2529=VERTEX_POINT('',#8766);
#2530=VERTEX_POINT('',#8770);
#2531=VERTEX_POINT('',#8772);
#2532=VERTEX_POINT('',#8776);
#2533=VERTEX_POINT('',#8778);
#2534=VERTEX_POINT('',#8780);
#2535=VERTEX_POINT('',#8784);
#2536=VERTEX_POINT('',#8786);
#2537=VERTEX_POINT('',#8788);
#2538=VERTEX_POINT('',#8790);
#2539=VERTEX_POINT('',#8792);
#2540=VERTEX_POINT('',#8794);
#2541=VERTEX_POINT('',#8796);
#2542=VERTEX_POINT('',#8800);
#2543=VERTEX_POINT('',#8804);
#2544=VERTEX_POINT('',#8808);
#2545=VERTEX_POINT('',#8809);
#2546=VERTEX_POINT('',#8811);
#2547=VERTEX_POINT('',#8813);
#2548=VERTEX_POINT('',#8817);
#2549=VERTEX_POINT('',#8818);
#2550=VERTEX_POINT('',#8820);
#2551=VERTEX_POINT('',#8822);
#2552=VERTEX_POINT('',#8826);
#2553=VERTEX_POINT('',#8828);
#2554=VERTEX_POINT('',#8832);
#2555=VERTEX_POINT('',#8833);
#2556=VERTEX_POINT('',#8835);
#2557=VERTEX_POINT('',#8837);
#2558=VERTEX_POINT('',#8841);
#2559=VERTEX_POINT('',#8843);
#2560=VERTEX_POINT('',#8850);
#2561=VERTEX_POINT('',#8852);
#2562=VERTEX_POINT('',#8856);
#2563=VERTEX_POINT('',#8858);
#2564=VERTEX_POINT('',#8865);
#2565=VERTEX_POINT('',#8867);
#2566=VERTEX_POINT('',#8871);
#2567=VERTEX_POINT('',#8873);
#2568=VERTEX_POINT('',#8880);
#2569=VERTEX_POINT('',#8885);
#2570=VERTEX_POINT('',#8889);
#2571=VERTEX_POINT('',#8893);
#2572=VERTEX_POINT('',#8897);
#2573=VERTEX_POINT('',#8901);
#2574=VERTEX_POINT('',#8906);
#2575=VERTEX_POINT('',#8910);
#2576=VERTEX_POINT('',#8942);
#2577=VERTEX_POINT('',#8943);
#2578=VERTEX_POINT('',#8945);
#2579=VERTEX_POINT('',#8947);
#2580=VERTEX_POINT('',#8951);
#2581=VERTEX_POINT('',#8952);
#2582=VERTEX_POINT('',#8954);
#2583=VERTEX_POINT('',#8956);
#2584=VERTEX_POINT('',#8960);
#2585=VERTEX_POINT('',#8962);
#2586=VERTEX_POINT('',#8966);
#2587=VERTEX_POINT('',#8968);
#2588=VERTEX_POINT('',#8972);
#2589=VERTEX_POINT('',#8974);
#2590=VERTEX_POINT('',#8978);
#2591=VERTEX_POINT('',#8980);
#2592=VERTEX_POINT('',#8984);
#2593=VERTEX_POINT('',#8986);
#2594=VERTEX_POINT('',#8990);
#2595=VERTEX_POINT('',#8992);
#2596=VERTEX_POINT('',#8996);
#2597=VERTEX_POINT('',#8998);
#2598=VERTEX_POINT('',#9002);
#2599=VERTEX_POINT('',#9004);
#2600=VERTEX_POINT('',#9014);
#2601=VERTEX_POINT('',#9016);
#2602=VERTEX_POINT('',#9020);
#2603=VERTEX_POINT('',#9024);
#2604=VERTEX_POINT('',#9028);
#2605=VERTEX_POINT('',#9032);
#2606=VERTEX_POINT('',#9036);
#2607=VERTEX_POINT('',#9041);
#2608=VERTEX_POINT('',#9042);
#2609=VERTEX_POINT('',#9047);
#2610=VERTEX_POINT('',#9051);
#2611=VERTEX_POINT('',#9055);
#2612=VERTEX_POINT('',#9059);
#2613=VERTEX_POINT('',#9061);
#2614=VERTEX_POINT('',#9065);
#2615=VERTEX_POINT('',#9067);
#2616=VERTEX_POINT('',#9071);
#2617=VERTEX_POINT('',#9073);
#2618=VERTEX_POINT('',#9077);
#2619=VERTEX_POINT('',#9079);
#2620=VERTEX_POINT('',#9083);
#2621=VERTEX_POINT('',#9085);
#2622=VERTEX_POINT('',#9090);
#2623=VERTEX_POINT('',#9094);
#2624=VERTEX_POINT('',#9113);
#2625=VERTEX_POINT('',#9115);
#2626=VERTEX_POINT('',#9119);
#2627=VERTEX_POINT('',#9121);
#2628=VERTEX_POINT('',#9125);
#2629=VERTEX_POINT('',#9127);
#2630=VERTEX_POINT('',#9131);
#2631=VERTEX_POINT('',#9133);
#2632=VERTEX_POINT('',#9137);
#2633=VERTEX_POINT('',#9139);
#2634=VERTEX_POINT('',#9143);
#2635=VERTEX_POINT('',#9145);
#2636=VERTEX_POINT('',#9149);
#2637=VERTEX_POINT('',#9151);
#2638=VERTEX_POINT('',#9155);
#2639=VERTEX_POINT('',#9157);
#2640=VERTEX_POINT('',#9161);
#2641=VERTEX_POINT('',#9163);
#2642=VERTEX_POINT('',#9167);
#2643=VERTEX_POINT('',#9169);
#2644=VERTEX_POINT('',#9173);
#2645=VERTEX_POINT('',#9174);
#2646=VERTEX_POINT('',#9176);
#2647=VERTEX_POINT('',#9178);
#2648=VERTEX_POINT('',#9182);
#2649=VERTEX_POINT('',#9184);
#2650=VERTEX_POINT('',#9188);
#2651=VERTEX_POINT('',#9190);
#2652=VERTEX_POINT('',#9194);
#2653=VERTEX_POINT('',#9196);
#2654=VERTEX_POINT('',#9200);
#2655=VERTEX_POINT('',#9202);
#2656=VERTEX_POINT('',#9206);
#2657=VERTEX_POINT('',#9208);
#2658=VERTEX_POINT('',#9212);
#2659=VERTEX_POINT('',#9214);
#2660=VERTEX_POINT('',#9221);
#2661=VERTEX_POINT('',#9223);
#2662=VERTEX_POINT('',#9227);
#2663=VERTEX_POINT('',#9231);
#2664=VERTEX_POINT('',#9235);
#2665=VERTEX_POINT('',#9240);
#2666=VERTEX_POINT('',#9241);
#2667=VERTEX_POINT('',#9246);
#2668=VERTEX_POINT('',#9250);
#2669=VERTEX_POINT('',#9254);
#2670=VERTEX_POINT('',#9258);
#2671=VERTEX_POINT('',#9260);
#2672=VERTEX_POINT('',#9264);
#2673=VERTEX_POINT('',#9266);
#2674=VERTEX_POINT('',#9270);
#2675=VERTEX_POINT('',#9272);
#2676=VERTEX_POINT('',#9288);
#2677=VERTEX_POINT('',#9290);
#2678=VERTEX_POINT('',#9294);
#2679=VERTEX_POINT('',#9296);
#2680=VERTEX_POINT('',#9300);
#2681=VERTEX_POINT('',#9301);
#2682=VERTEX_POINT('',#9303);
#2683=VERTEX_POINT('',#9305);
#2684=VERTEX_POINT('',#9307);
#2685=VERTEX_POINT('',#9309);
#2686=VERTEX_POINT('',#9311);
#2687=VERTEX_POINT('',#9313);
#2688=VERTEX_POINT('',#9317);
#2689=VERTEX_POINT('',#9319);
#2690=VERTEX_POINT('',#9323);
#2691=VERTEX_POINT('',#9327);
#2692=VERTEX_POINT('',#9331);
#2693=VERTEX_POINT('',#9335);
#2694=VERTEX_POINT('',#9339);
#2695=VERTEX_POINT('',#9343);
#2696=VERTEX_POINT('',#9351);
#2697=VERTEX_POINT('',#9353);
#2698=VERTEX_POINT('',#9358);
#2699=VERTEX_POINT('',#9360);
#2700=VERTEX_POINT('',#9365);
#2701=VERTEX_POINT('',#9367);
#2702=VERTEX_POINT('',#9372);
#2703=VERTEX_POINT('',#9373);
#2704=VERTEX_POINT('',#9375);
#2705=VERTEX_POINT('',#9377);
#2706=VERTEX_POINT('',#9381);
#2707=VERTEX_POINT('',#9383);
#2708=VERTEX_POINT('',#9387);
#2709=VERTEX_POINT('',#9389);
#2710=VERTEX_POINT('',#9396);
#2711=VERTEX_POINT('',#9398);
#2712=VERTEX_POINT('',#9400);
#2713=VERTEX_POINT('',#9402);
#2714=VERTEX_POINT('',#9406);
#2715=VERTEX_POINT('',#9408);
#2716=VERTEX_POINT('',#9410);
#2717=VERTEX_POINT('',#9412);
#2718=VERTEX_POINT('',#9414);
#2719=VERTEX_POINT('',#9416);
#2720=VERTEX_POINT('',#9418);
#2721=VERTEX_POINT('',#9420);
#2722=VERTEX_POINT('',#9422);
#2723=VERTEX_POINT('',#9427);
#2724=VERTEX_POINT('',#9429);
#2725=VERTEX_POINT('',#9431);
#2726=VERTEX_POINT('',#9435);
#2727=VERTEX_POINT('',#9437);
#2728=VERTEX_POINT('',#9439);
#2729=VERTEX_POINT('',#9441);
#2730=VERTEX_POINT('',#9443);
#2731=VERTEX_POINT('',#9445);
#2732=VERTEX_POINT('',#9447);
#2733=VERTEX_POINT('',#9449);
#2734=VERTEX_POINT('',#9453);
#2735=VERTEX_POINT('',#9457);
#2736=VERTEX_POINT('',#9461);
#2737=VERTEX_POINT('',#9467);
#2738=VERTEX_POINT('',#9468);
#2739=VERTEX_POINT('',#9473);
#2740=VERTEX_POINT('',#9477);
#2741=VERTEX_POINT('',#9481);
#2742=VERTEX_POINT('',#9485);
#2743=VERTEX_POINT('',#9493);
#2744=VERTEX_POINT('',#9495);
#2745=VERTEX_POINT('',#9499);
#2746=VERTEX_POINT('',#9503);
#2747=VERTEX_POINT('',#9507);
#2748=VERTEX_POINT('',#9520);
#2749=VERTEX_POINT('',#9524);
#2750=VERTEX_POINT('',#9539);
#2751=VERTEX_POINT('',#9541);
#2752=VERTEX_POINT('',#9545);
#2753=VERTEX_POINT('',#9547);
#2754=VERTEX_POINT('',#9551);
#2755=VERTEX_POINT('',#9553);
#2756=VERTEX_POINT('',#9557);
#2757=VERTEX_POINT('',#9559);
#2758=VERTEX_POINT('',#9563);
#2759=VERTEX_POINT('',#9564);
#2760=VERTEX_POINT('',#9566);
#2761=VERTEX_POINT('',#9568);
#2762=VERTEX_POINT('',#9572);
#2763=VERTEX_POINT('',#9573);
#2764=VERTEX_POINT('',#9575);
#2765=VERTEX_POINT('',#9577);
#2766=VERTEX_POINT('',#9581);
#2767=VERTEX_POINT('',#9583);
#2768=VERTEX_POINT('',#9587);
#2769=VERTEX_POINT('',#9588);
#2770=VERTEX_POINT('',#9590);
#2771=VERTEX_POINT('',#9592);
#2772=VERTEX_POINT('',#9596);
#2773=VERTEX_POINT('',#9598);
#2774=VERTEX_POINT('',#9605);
#2775=VERTEX_POINT('',#9607);
#2776=VERTEX_POINT('',#9611);
#2777=VERTEX_POINT('',#9613);
#2778=VERTEX_POINT('',#9620);
#2779=VERTEX_POINT('',#9622);
#2780=VERTEX_POINT('',#9626);
#2781=VERTEX_POINT('',#9628);
#2782=VERTEX_POINT('',#9635);
#2783=VERTEX_POINT('',#9637);
#2784=VERTEX_POINT('',#9641);
#2785=VERTEX_POINT('',#9645);
#2786=VERTEX_POINT('',#9649);
#2787=VERTEX_POINT('',#9653);
#2788=VERTEX_POINT('',#9657);
#2789=VERTEX_POINT('',#9662);
#2790=VERTEX_POINT('',#9663);
#2791=VERTEX_POINT('',#9665);
#2792=VERTEX_POINT('',#9667);
#2793=VERTEX_POINT('',#9671);
#2794=VERTEX_POINT('',#9673);
#2795=VERTEX_POINT('',#9677);
#2796=VERTEX_POINT('',#9679);
#2797=VERTEX_POINT('',#9683);
#2798=VERTEX_POINT('',#9685);
#2799=VERTEX_POINT('',#9689);
#2800=VERTEX_POINT('',#9694);
#2801=VERTEX_POINT('',#9698);
#2802=VERTEX_POINT('',#9702);
#2803=VERTEX_POINT('',#9706);
#2804=VERTEX_POINT('',#9710);
#2805=VERTEX_POINT('',#9714);
#2806=VERTEX_POINT('',#9734);
#2807=VERTEX_POINT('',#9736);
#2808=VERTEX_POINT('',#9740);
#2809=VERTEX_POINT('',#9742);
#2810=VERTEX_POINT('',#9746);
#2811=VERTEX_POINT('',#9748);
#2812=VERTEX_POINT('',#9752);
#2813=VERTEX_POINT('',#9754);
#2814=VERTEX_POINT('',#9758);
#2815=VERTEX_POINT('',#9759);
#2816=VERTEX_POINT('',#9761);
#2817=VERTEX_POINT('',#9763);
#2818=VERTEX_POINT('',#9767);
#2819=VERTEX_POINT('',#9768);
#2820=VERTEX_POINT('',#9770);
#2821=VERTEX_POINT('',#9772);
#2822=VERTEX_POINT('',#9776);
#2823=VERTEX_POINT('',#9778);
#2824=VERTEX_POINT('',#9782);
#2825=VERTEX_POINT('',#9783);
#2826=VERTEX_POINT('',#9785);
#2827=VERTEX_POINT('',#9787);
#2828=VERTEX_POINT('',#9791);
#2829=VERTEX_POINT('',#9793);
#2830=VERTEX_POINT('',#9800);
#2831=VERTEX_POINT('',#9802);
#2832=VERTEX_POINT('',#9806);
#2833=VERTEX_POINT('',#9808);
#2834=VERTEX_POINT('',#9815);
#2835=VERTEX_POINT('',#9817);
#2836=VERTEX_POINT('',#9821);
#2837=VERTEX_POINT('',#9823);
#2838=VERTEX_POINT('',#9830);
#2839=VERTEX_POINT('',#9832);
#2840=VERTEX_POINT('',#9836);
#2841=VERTEX_POINT('',#9840);
#2842=VERTEX_POINT('',#9844);
#2843=VERTEX_POINT('',#9848);
#2844=VERTEX_POINT('',#9852);
#2845=VERTEX_POINT('',#9857);
#2846=VERTEX_POINT('',#9858);
#2847=VERTEX_POINT('',#9860);
#2848=VERTEX_POINT('',#9862);
#2849=VERTEX_POINT('',#9866);
#2850=VERTEX_POINT('',#9868);
#2851=VERTEX_POINT('',#9872);
#2852=VERTEX_POINT('',#9874);
#2853=VERTEX_POINT('',#9878);
#2854=VERTEX_POINT('',#9880);
#2855=VERTEX_POINT('',#9884);
#2856=VERTEX_POINT('',#9889);
#2857=VERTEX_POINT('',#9893);
#2858=VERTEX_POINT('',#9897);
#2859=VERTEX_POINT('',#9901);
#2860=VERTEX_POINT('',#9905);
#2861=VERTEX_POINT('',#9909);
#2862=VERTEX_POINT('',#9929);
#2863=VERTEX_POINT('',#9930);
#2864=VERTEX_POINT('',#9932);
#2865=VERTEX_POINT('',#9934);
#2866=VERTEX_POINT('',#9938);
#2867=VERTEX_POINT('',#9939);
#2868=VERTEX_POINT('',#9941);
#2869=VERTEX_POINT('',#9943);
#2870=VERTEX_POINT('',#9947);
#2871=VERTEX_POINT('',#9949);
#2872=VERTEX_POINT('',#9953);
#2873=VERTEX_POINT('',#9955);
#2874=VERTEX_POINT('',#9959);
#2875=VERTEX_POINT('',#9961);
#2876=VERTEX_POINT('',#9965);
#2877=VERTEX_POINT('',#9967);
#2878=VERTEX_POINT('',#9971);
#2879=VERTEX_POINT('',#9973);
#2880=VERTEX_POINT('',#9977);
#2881=VERTEX_POINT('',#9979);
#2882=VERTEX_POINT('',#9983);
#2883=VERTEX_POINT('',#9985);
#2884=VERTEX_POINT('',#9989);
#2885=VERTEX_POINT('',#9991);
#2886=VERTEX_POINT('',#10001);
#2887=VERTEX_POINT('',#10003);
#2888=VERTEX_POINT('',#10007);
#2889=VERTEX_POINT('',#10011);
#2890=VERTEX_POINT('',#10015);
#2891=VERTEX_POINT('',#10019);
#2892=VERTEX_POINT('',#10023);
#2893=VERTEX_POINT('',#10028);
#2894=VERTEX_POINT('',#10029);
#2895=VERTEX_POINT('',#10034);
#2896=VERTEX_POINT('',#10038);
#2897=VERTEX_POINT('',#10042);
#2898=VERTEX_POINT('',#10046);
#2899=VERTEX_POINT('',#10048);
#2900=VERTEX_POINT('',#10052);
#2901=VERTEX_POINT('',#10054);
#2902=VERTEX_POINT('',#10058);
#2903=VERTEX_POINT('',#10060);
#2904=VERTEX_POINT('',#10064);
#2905=VERTEX_POINT('',#10066);
#2906=VERTEX_POINT('',#10070);
#2907=VERTEX_POINT('',#10072);
#2908=VERTEX_POINT('',#10077);
#2909=VERTEX_POINT('',#10081);
#2910=EDGE_CURVE('',#2430,#2430,#2334,.T.);
#2911=EDGE_CURVE('',#2430,#2431,#1234,.T.);
#2912=EDGE_CURVE('',#2431,#2431,#2335,.T.);
#2913=EDGE_CURVE('',#2432,#2432,#2336,.T.);
#2914=EDGE_CURVE('',#2432,#2433,#1235,.T.);
#2915=EDGE_CURVE('',#2433,#2433,#2337,.T.);
#2916=EDGE_CURVE('',#2434,#2434,#2338,.T.);
#2917=EDGE_CURVE('',#2434,#2435,#1236,.T.);
#2918=EDGE_CURVE('',#2435,#2435,#2339,.T.);
#2919=EDGE_CURVE('',#2436,#2436,#2340,.T.);
#2920=EDGE_CURVE('',#2436,#2437,#1237,.T.);
#2921=EDGE_CURVE('',#2437,#2437,#2341,.T.);
#2922=EDGE_CURVE('',#2438,#2438,#2342,.T.);
#2923=EDGE_CURVE('',#2438,#2439,#1238,.T.);
#2924=EDGE_CURVE('',#2439,#2439,#2343,.T.);
#2925=EDGE_CURVE('',#2440,#2440,#2344,.T.);
#2926=EDGE_CURVE('',#2440,#2441,#1239,.T.);
#2927=EDGE_CURVE('',#2441,#2441,#2345,.T.);
#2928=EDGE_CURVE('',#2442,#2442,#2346,.T.);
#2929=EDGE_CURVE('',#2442,#2443,#1240,.T.);
#2930=EDGE_CURVE('',#2443,#2443,#2347,.T.);
#2931=EDGE_CURVE('',#2444,#2444,#2348,.T.);
#2932=EDGE_CURVE('',#2444,#2445,#1241,.T.);
#2933=EDGE_CURVE('',#2445,#2445,#2349,.T.);
#2934=EDGE_CURVE('',#2446,#2447,#2350,.T.);
#2935=EDGE_CURVE('',#2447,#2448,#1242,.T.);
#2936=EDGE_CURVE('',#2448,#2449,#2351,.T.);
#2937=EDGE_CURVE('',#2449,#2446,#1243,.T.);
#2938=EDGE_CURVE('',#2450,#2449,#1244,.T.);
#2939=EDGE_CURVE('',#2451,#2450,#1245,.T.);
#2940=EDGE_CURVE('',#2446,#2451,#1246,.T.);
#2941=EDGE_CURVE('',#2448,#2452,#1247,.T.);
#2942=EDGE_CURVE('',#2453,#2452,#2352,.T.);
#2943=EDGE_CURVE('',#2453,#2454,#1248,.T.);
#2944=EDGE_CURVE('',#2455,#2454,#2353,.T.);
#2945=EDGE_CURVE('',#2455,#2456,#1249,.T.);
#2946=EDGE_CURVE('',#2450,#2456,#2354,.T.);
#2947=EDGE_CURVE('',#2457,#2458,#2355,.T.);
#2948=EDGE_CURVE('',#2458,#2453,#1250,.T.);
#2949=EDGE_CURVE('',#2452,#2457,#1251,.T.);
#2950=EDGE_CURVE('',#2459,#2458,#1252,.T.);
#2951=EDGE_CURVE('',#2454,#2459,#1253,.T.);
#2952=EDGE_CURVE('',#2459,#2460,#2356,.T.);
#2953=EDGE_CURVE('',#2460,#2455,#1254,.T.);
#2954=EDGE_CURVE('',#2461,#2451,#2357,.T.);
#2955=EDGE_CURVE('',#2456,#2461,#1255,.T.);
#2956=EDGE_CURVE('',#2461,#2460,#1256,.T.);
#2957=EDGE_CURVE('',#2457,#2447,#1257,.T.);
#2958=EDGE_CURVE('',#2462,#2462,#2358,.T.);
#2959=EDGE_CURVE('',#2462,#2463,#1258,.T.);
#2960=EDGE_CURVE('',#2463,#2463,#2359,.T.);
#2961=EDGE_CURVE('',#2464,#2465,#1259,.T.);
#2962=EDGE_CURVE('',#2465,#2466,#1260,.T.);
#2963=EDGE_CURVE('',#2466,#2467,#1261,.T.);
#2964=EDGE_CURVE('',#2464,#2467,#1262,.T.);
#2965=EDGE_CURVE('',#2465,#2468,#1263,.T.);
#2966=EDGE_CURVE('',#2468,#2469,#1264,.T.);
#2967=EDGE_CURVE('',#2469,#2466,#1265,.T.);
#2968=EDGE_CURVE('',#2468,#2470,#1266,.T.);
#2969=EDGE_CURVE('',#2470,#2471,#1267,.T.);
#2970=EDGE_CURVE('',#2471,#2469,#1268,.T.);
#2971=EDGE_CURVE('',#2470,#2472,#1269,.T.);
#2972=EDGE_CURVE('',#2472,#2473,#1270,.T.);
#2973=EDGE_CURVE('',#2473,#2471,#1271,.T.);
#2974=EDGE_CURVE('',#2472,#2474,#1272,.T.);
#2975=EDGE_CURVE('',#2474,#2475,#1273,.T.);
#2976=EDGE_CURVE('',#2475,#2473,#1274,.T.);
#2977=EDGE_CURVE('',#2476,#2475,#1275,.T.);
#2978=EDGE_CURVE('',#2474,#2477,#1276,.T.);
#2979=EDGE_CURVE('',#2477,#2476,#1277,.T.);
#2980=EDGE_CURVE('',#2478,#2476,#1278,.T.);
#2981=EDGE_CURVE('',#2477,#2479,#1279,.T.);
#2982=EDGE_CURVE('',#2479,#2478,#1280,.T.);
#2983=EDGE_CURVE('',#2480,#2478,#1281,.T.);
#2984=EDGE_CURVE('',#2479,#2481,#1282,.T.);
#2985=EDGE_CURVE('',#2481,#2480,#1283,.T.);
#2986=EDGE_CURVE('',#2482,#2480,#1284,.T.);
#2987=EDGE_CURVE('',#2481,#2483,#1285,.T.);
#2988=EDGE_CURVE('',#2483,#2482,#1286,.T.);
#2989=EDGE_CURVE('',#2484,#2482,#1287,.T.);
#2990=EDGE_CURVE('',#2483,#2485,#1288,.T.);
#2991=EDGE_CURVE('',#2485,#2484,#1289,.T.);
#2992=EDGE_CURVE('',#2486,#2484,#1290,.T.);
#2993=EDGE_CURVE('',#2485,#2487,#1291,.T.);
#2994=EDGE_CURVE('',#2487,#2486,#1292,.T.);
#2995=EDGE_CURVE('',#2467,#2486,#1293,.T.);
#2996=EDGE_CURVE('',#2487,#2464,#1294,.T.);
#2997=EDGE_CURVE('',#2480,#2488,#1295,.T.);
#2998=EDGE_CURVE('',#2488,#2489,#1296,.T.);
#2999=EDGE_CURVE('',#2489,#2478,#1297,.T.);
#3000=EDGE_CURVE('',#2490,#2482,#1298,.T.);
#3001=EDGE_CURVE('',#2490,#2488,#1299,.T.);
#3002=EDGE_CURVE('',#2484,#2491,#1300,.T.);
#3003=EDGE_CURVE('',#2491,#2490,#1301,.T.);
#3004=EDGE_CURVE('',#2492,#2486,#1302,.T.);
#3005=EDGE_CURVE('',#2492,#2491,#1303,.T.);
#3006=EDGE_CURVE('',#2467,#2493,#1304,.T.);
#3007=EDGE_CURVE('',#2493,#2492,#1305,.T.);
#3008=EDGE_CURVE('',#2494,#2466,#1306,.T.);
#3009=EDGE_CURVE('',#2494,#2493,#1307,.T.);
#3010=EDGE_CURVE('',#2476,#2495,#1308,.T.);
#3011=EDGE_CURVE('',#2495,#2496,#1309,.T.);
#3012=EDGE_CURVE('',#2496,#2475,#1310,.T.);
#3013=EDGE_CURVE('',#2496,#2497,#1311,.T.);
#3014=EDGE_CURVE('',#2473,#2497,#1312,.T.);
#3015=EDGE_CURVE('',#2489,#2495,#1313,.T.);
#3016=EDGE_CURVE('',#2498,#2494,#1314,.T.);
#3017=EDGE_CURVE('',#2499,#2498,#1315,.T.);
#3018=EDGE_CURVE('',#2497,#2499,#1316,.T.);
#3019=EDGE_CURVE('',#2499,#2471,#1317,.T.);
#3020=EDGE_CURVE('',#2469,#2498,#1318,.T.);
#3021=EDGE_CURVE('',#2500,#2501,#2360,.T.);
#3022=EDGE_CURVE('',#2501,#2502,#2361,.T.);
#3023=EDGE_CURVE('',#2502,#2503,#207,.T.);
#3024=EDGE_CURVE('',#2503,#2500,#2362,.T.);
#3025=EDGE_CURVE('',#2504,#2505,#2363,.T.);
#3026=EDGE_CURVE('',#2505,#2501,#1319,.T.);
#3027=EDGE_CURVE('',#2500,#2504,#1320,.T.);
#3028=EDGE_CURVE('',#2506,#2507,#208,.T.);
#3029=EDGE_CURVE('',#2507,#2505,#2364,.T.);
#3030=EDGE_CURVE('',#2504,#2506,#2365,.T.);
#3031=EDGE_CURVE('',#2503,#2508,#1321,.T.);
#3032=EDGE_CURVE('',#2508,#2509,#1322,.T.);
#3033=EDGE_CURVE('',#2509,#2506,#1323,.T.);
#3034=EDGE_CURVE('',#2510,#2511,#2366,.T.);
#3035=EDGE_CURVE('',#2511,#2512,#2367,.T.);
#3036=EDGE_CURVE('',#2512,#2513,#209,.T.);
#3037=EDGE_CURVE('',#2513,#2510,#2368,.T.);
#3038=EDGE_CURVE('',#2514,#2515,#2369,.T.);
#3039=EDGE_CURVE('',#2515,#2511,#1324,.T.);
#3040=EDGE_CURVE('',#2510,#2514,#1325,.T.);
#3041=EDGE_CURVE('',#2516,#2517,#210,.T.);
#3042=EDGE_CURVE('',#2517,#2515,#2370,.T.);
#3043=EDGE_CURVE('',#2514,#2516,#2371,.T.);
#3044=EDGE_CURVE('',#2513,#2518,#1326,.T.);
#3045=EDGE_CURVE('',#2518,#2519,#1327,.T.);
#3046=EDGE_CURVE('',#2519,#2516,#1328,.T.);
#3047=EDGE_CURVE('',#2520,#2520,#2372,.T.);
#3048=EDGE_CURVE('',#2520,#2521,#1329,.T.);
#3049=EDGE_CURVE('',#2521,#2521,#2373,.T.);
#3050=EDGE_CURVE('',#2522,#2522,#2374,.T.);
#3051=EDGE_CURVE('',#2522,#2523,#1330,.T.);
#3052=EDGE_CURVE('',#2523,#2523,#2375,.T.);
#3053=EDGE_CURVE('',#2524,#2524,#2376,.T.);
#3054=EDGE_CURVE('',#2524,#2525,#1331,.T.);
#3055=EDGE_CURVE('',#2525,#2525,#2377,.T.);
#3056=EDGE_CURVE('',#2526,#2526,#2378,.T.);
#3057=EDGE_CURVE('',#2526,#2527,#1332,.T.);
#3058=EDGE_CURVE('',#2527,#2527,#2379,.T.);
#3059=EDGE_CURVE('',#2508,#2519,#1333,.T.);
#3060=EDGE_CURVE('',#2509,#2518,#1334,.T.);
#3061=EDGE_CURVE('',#2507,#2528,#1335,.T.);
#3062=EDGE_CURVE('',#2529,#2528,#51,.T.);
#3063=EDGE_CURVE('',#2529,#2505,#1336,.T.);
#3064=EDGE_CURVE('',#2511,#2530,#1337,.T.);
#3065=EDGE_CURVE('',#2530,#2531,#52,.T.);
#3066=EDGE_CURVE('',#2531,#2512,#1338,.T.);
#3067=EDGE_CURVE('',#2532,#2529,#1339,.T.);
#3068=EDGE_CURVE('',#2533,#2532,#1340,.T.);
#3069=EDGE_CURVE('',#2534,#2533,#1341,.T.);
#3070=EDGE_CURVE('',#2501,#2534,#1342,.T.);
#3071=EDGE_CURVE('',#2535,#2515,#1343,.T.);
#3072=EDGE_CURVE('',#2536,#2535,#1344,.T.);
#3073=EDGE_CURVE('',#2537,#2536,#1345,.T.);
#3074=EDGE_CURVE('',#2538,#2537,#1346,.T.);
#3075=EDGE_CURVE('',#2539,#2538,#1347,.T.);
#3076=EDGE_CURVE('',#2540,#2539,#1348,.T.);
#3077=EDGE_CURVE('',#2541,#2540,#1349,.T.);
#3078=EDGE_CURVE('',#2530,#2541,#1350,.T.);
#3079=EDGE_CURVE('',#2534,#2542,#53,.T.);
#3080=EDGE_CURVE('',#2542,#2502,#1351,.T.);
#3081=EDGE_CURVE('',#2517,#2543,#1352,.T.);
#3082=EDGE_CURVE('',#2535,#2543,#54,.T.);
#3083=EDGE_CURVE('',#2544,#2545,#1353,.T.);
#3084=EDGE_CURVE('',#2545,#2546,#55,.T.);
#3085=EDGE_CURVE('',#2546,#2547,#1354,.T.);
#3086=EDGE_CURVE('',#2544,#2547,#56,.T.);
#3087=EDGE_CURVE('',#2548,#2549,#1355,.T.);
#3088=EDGE_CURVE('',#2549,#2550,#57,.T.);
#3089=EDGE_CURVE('',#2550,#2551,#1356,.T.);
#3090=EDGE_CURVE('',#2551,#2548,#58,.T.);
#3091=EDGE_CURVE('',#2549,#2552,#1357,.T.);
#3092=EDGE_CURVE('',#2552,#2553,#59,.T.);
#3093=EDGE_CURVE('',#2553,#2550,#1358,.T.);
#3094=EDGE_CURVE('',#2554,#2555,#1359,.T.);
#3095=EDGE_CURVE('',#2555,#2556,#60,.T.);
#3096=EDGE_CURVE('',#2556,#2557,#1360,.T.);
#3097=EDGE_CURVE('',#2557,#2554,#61,.T.);
#3098=EDGE_CURVE('',#2552,#2558,#1361,.T.);
#3099=EDGE_CURVE('',#2558,#2559,#62,.T.);
#3100=EDGE_CURVE('',#2559,#2553,#1362,.T.);
#3101=EDGE_CURVE('',#2555,#2559,#1363,.T.);
#3102=EDGE_CURVE('',#2558,#2556,#1364,.T.);
#3103=EDGE_CURVE('',#2560,#2554,#1365,.T.);
#3104=EDGE_CURVE('',#2557,#2561,#1366,.T.);
#3105=EDGE_CURVE('',#2561,#2560,#63,.T.);
#3106=EDGE_CURVE('',#2562,#2560,#1367,.T.);
#3107=EDGE_CURVE('',#2561,#2563,#1368,.T.);
#3108=EDGE_CURVE('',#2563,#2562,#64,.T.);
#3109=EDGE_CURVE('',#2545,#2548,#1369,.T.);
#3110=EDGE_CURVE('',#2551,#2546,#1370,.T.);
#3111=EDGE_CURVE('',#2564,#2562,#1371,.T.);
#3112=EDGE_CURVE('',#2563,#2565,#1372,.T.);
#3113=EDGE_CURVE('',#2565,#2564,#65,.T.);
#3114=EDGE_CURVE('',#2566,#2564,#1373,.T.);
#3115=EDGE_CURVE('',#2565,#2567,#1374,.T.);
#3116=EDGE_CURVE('',#2567,#2566,#66,.T.);
#3117=EDGE_CURVE('',#2547,#2566,#1375,.T.);
#3118=EDGE_CURVE('',#2567,#2544,#1376,.T.);
#3119=EDGE_CURVE('',#2551,#2568,#1377,.T.);
#3120=EDGE_CURVE('',#2543,#2568,#1378,.T.);
#3121=EDGE_CURVE('',#2543,#2546,#1379,.T.);
#3122=EDGE_CURVE('',#2550,#2569,#1380,.T.);
#3123=EDGE_CURVE('',#2568,#2569,#1381,.T.);
#3124=EDGE_CURVE('',#2553,#2570,#1382,.T.);
#3125=EDGE_CURVE('',#2569,#2570,#1383,.T.);
#3126=EDGE_CURVE('',#2571,#2559,#1384,.T.);
#3127=EDGE_CURVE('',#2570,#2571,#1385,.T.);
#3128=EDGE_CURVE('',#2555,#2572,#1386,.T.);
#3129=EDGE_CURVE('',#2571,#2572,#1387,.T.);
#3130=EDGE_CURVE('',#2554,#2573,#1388,.T.);
#3131=EDGE_CURVE('',#2572,#2573,#1389,.T.);
#3132=EDGE_CURVE('',#2533,#2574,#67,.T.);
#3133=EDGE_CURVE('',#2574,#2542,#1390,.T.);
#3134=EDGE_CURVE('',#2532,#2575,#68,.T.);
#3135=EDGE_CURVE('',#2575,#2574,#1391,.T.);
#3136=EDGE_CURVE('',#2528,#2575,#1392,.T.);
#3137=EDGE_CURVE('',#2541,#2573,#69,.T.);
#3138=EDGE_CURVE('',#2573,#2531,#1393,.T.);
#3139=EDGE_CURVE('',#2540,#2572,#70,.T.);
#3140=EDGE_CURVE('',#2539,#2571,#71,.T.);
#3141=EDGE_CURVE('',#2538,#2570,#72,.T.);
#3142=EDGE_CURVE('',#2537,#2569,#73,.T.);
#3143=EDGE_CURVE('',#2536,#2568,#74,.T.);
#3144=EDGE_CURVE('',#2547,#2542,#1394,.T.);
#3145=EDGE_CURVE('',#2566,#2574,#1395,.T.);
#3146=EDGE_CURVE('',#2564,#2575,#1396,.T.);
#3147=EDGE_CURVE('',#2562,#2528,#1397,.T.);
#3148=EDGE_CURVE('',#2560,#2531,#1398,.T.);
#3149=EDGE_CURVE('',#2576,#2577,#1399,.T.);
#3150=EDGE_CURVE('',#2577,#2578,#75,.T.);
#3151=EDGE_CURVE('',#2578,#2579,#1400,.T.);
#3152=EDGE_CURVE('',#2579,#2576,#76,.T.);
#3153=EDGE_CURVE('',#2580,#2581,#1401,.T.);
#3154=EDGE_CURVE('',#2581,#2582,#77,.T.);
#3155=EDGE_CURVE('',#2582,#2583,#1402,.T.);
#3156=EDGE_CURVE('',#2583,#2580,#78,.T.);
#3157=EDGE_CURVE('',#2581,#2584,#1403,.T.);
#3158=EDGE_CURVE('',#2584,#2585,#79,.T.);
#3159=EDGE_CURVE('',#2585,#2582,#1404,.T.);
#3160=EDGE_CURVE('',#2584,#2586,#1405,.T.);
#3161=EDGE_CURVE('',#2586,#2587,#80,.T.);
#3162=EDGE_CURVE('',#2587,#2585,#1406,.T.);
#3163=EDGE_CURVE('',#2586,#2588,#1407,.T.);
#3164=EDGE_CURVE('',#2588,#2589,#81,.T.);
#3165=EDGE_CURVE('',#2589,#2587,#1408,.T.);
#3166=EDGE_CURVE('',#2588,#2590,#1409,.T.);
#3167=EDGE_CURVE('',#2590,#2591,#82,.T.);
#3168=EDGE_CURVE('',#2591,#2589,#1410,.T.);
#3169=EDGE_CURVE('',#2592,#2591,#1411,.T.);
#3170=EDGE_CURVE('',#2590,#2593,#1412,.T.);
#3171=EDGE_CURVE('',#2593,#2592,#83,.T.);
#3172=EDGE_CURVE('',#2594,#2592,#1413,.T.);
#3173=EDGE_CURVE('',#2593,#2595,#1414,.T.);
#3174=EDGE_CURVE('',#2595,#2594,#84,.T.);
#3175=EDGE_CURVE('',#2596,#2594,#1415,.T.);
#3176=EDGE_CURVE('',#2595,#2597,#1416,.T.);
#3177=EDGE_CURVE('',#2597,#2596,#85,.T.);
#3178=EDGE_CURVE('',#2598,#2596,#1417,.T.);
#3179=EDGE_CURVE('',#2597,#2599,#1418,.T.);
#3180=EDGE_CURVE('',#2599,#2598,#86,.T.);
#3181=EDGE_CURVE('',#2577,#2598,#1419,.T.);
#3182=EDGE_CURVE('',#2599,#2578,#1420,.T.);
#3183=EDGE_CURVE('',#2583,#2576,#1421,.T.);
#3184=EDGE_CURVE('',#2579,#2580,#1422,.T.);
#3185=EDGE_CURVE('',#2596,#2600,#1423,.T.);
#3186=EDGE_CURVE('',#2601,#2600,#1424,.T.);
#3187=EDGE_CURVE('',#2601,#2594,#1425,.T.);
#3188=EDGE_CURVE('',#2602,#2598,#1426,.T.);
#3189=EDGE_CURVE('',#2600,#2602,#1427,.T.);
#3190=EDGE_CURVE('',#2577,#2603,#1428,.T.);
#3191=EDGE_CURVE('',#2602,#2603,#1429,.T.);
#3192=EDGE_CURVE('',#2604,#2576,#1430,.T.);
#3193=EDGE_CURVE('',#2603,#2604,#1431,.T.);
#3194=EDGE_CURVE('',#2583,#2605,#1432,.T.);
#3195=EDGE_CURVE('',#2604,#2605,#1433,.T.);
#3196=EDGE_CURVE('',#2606,#2582,#1434,.T.);
#3197=EDGE_CURVE('',#2605,#2606,#1435,.T.);
#3198=EDGE_CURVE('',#2607,#2608,#1436,.T.);
#3199=EDGE_CURVE('',#2608,#2603,#87,.T.);
#3200=EDGE_CURVE('',#2607,#2604,#88,.T.);
#3201=EDGE_CURVE('',#2608,#2609,#1437,.T.);
#3202=EDGE_CURVE('',#2609,#2602,#89,.T.);
#3203=EDGE_CURVE('',#2609,#2610,#1438,.T.);
#3204=EDGE_CURVE('',#2610,#2600,#90,.T.);
#3205=EDGE_CURVE('',#2610,#2611,#1439,.T.);
#3206=EDGE_CURVE('',#2611,#2601,#91,.T.);
#3207=EDGE_CURVE('',#2611,#2612,#1440,.T.);
#3208=EDGE_CURVE('',#2612,#2613,#92,.T.);
#3209=EDGE_CURVE('',#2613,#2601,#1441,.T.);
#3210=EDGE_CURVE('',#2614,#2613,#1442,.T.);
#3211=EDGE_CURVE('',#2612,#2615,#1443,.T.);
#3212=EDGE_CURVE('',#2615,#2614,#93,.T.);
#3213=EDGE_CURVE('',#2616,#2614,#1444,.T.);
#3214=EDGE_CURVE('',#2615,#2617,#1445,.T.);
#3215=EDGE_CURVE('',#2617,#2616,#94,.T.);
#3216=EDGE_CURVE('',#2618,#2616,#1446,.T.);
#3217=EDGE_CURVE('',#2617,#2619,#1447,.T.);
#3218=EDGE_CURVE('',#2619,#2618,#95,.T.);
#3219=EDGE_CURVE('',#2620,#2618,#1448,.T.);
#3220=EDGE_CURVE('',#2619,#2621,#1449,.T.);
#3221=EDGE_CURVE('',#2621,#2620,#96,.T.);
#3222=EDGE_CURVE('',#2606,#2620,#1450,.T.);
#3223=EDGE_CURVE('',#2621,#2622,#1451,.T.);
#3224=EDGE_CURVE('',#2622,#2606,#97,.T.);
#3225=EDGE_CURVE('',#2622,#2623,#1452,.T.);
#3226=EDGE_CURVE('',#2623,#2605,#98,.T.);
#3227=EDGE_CURVE('',#2623,#2607,#1453,.T.);
#3228=EDGE_CURVE('',#2589,#2616,#1454,.T.);
#3229=EDGE_CURVE('',#2618,#2587,#1455,.T.);
#3230=EDGE_CURVE('',#2585,#2620,#1456,.T.);
#3231=EDGE_CURVE('',#2592,#2613,#1457,.T.);
#3232=EDGE_CURVE('',#2614,#2591,#1458,.T.);
#3233=EDGE_CURVE('',#2624,#2624,#2380,.T.);
#3234=EDGE_CURVE('',#2624,#2625,#1459,.T.);
#3235=EDGE_CURVE('',#2625,#2625,#2381,.T.);
#3236=EDGE_CURVE('',#2626,#2626,#2382,.T.);
#3237=EDGE_CURVE('',#2626,#2627,#1460,.T.);
#3238=EDGE_CURVE('',#2627,#2627,#2383,.T.);
#3239=EDGE_CURVE('',#2628,#2628,#2384,.T.);
#3240=EDGE_CURVE('',#2628,#2629,#1461,.T.);
#3241=EDGE_CURVE('',#2629,#2629,#2385,.T.);
#3242=EDGE_CURVE('',#2630,#2630,#2386,.T.);
#3243=EDGE_CURVE('',#2630,#2631,#1462,.T.);
#3244=EDGE_CURVE('',#2631,#2631,#2387,.T.);
#3245=EDGE_CURVE('',#2632,#2632,#2388,.T.);
#3246=EDGE_CURVE('',#2632,#2633,#1463,.T.);
#3247=EDGE_CURVE('',#2633,#2633,#2389,.T.);
#3248=EDGE_CURVE('',#2634,#2634,#2390,.T.);
#3249=EDGE_CURVE('',#2634,#2635,#1464,.T.);
#3250=EDGE_CURVE('',#2635,#2635,#2391,.T.);
#3251=EDGE_CURVE('',#2636,#2636,#2392,.T.);
#3252=EDGE_CURVE('',#2636,#2637,#1465,.T.);
#3253=EDGE_CURVE('',#2637,#2637,#2393,.T.);
#3254=EDGE_CURVE('',#2638,#2638,#2394,.T.);
#3255=EDGE_CURVE('',#2638,#2639,#1466,.T.);
#3256=EDGE_CURVE('',#2639,#2639,#2395,.T.);
#3257=EDGE_CURVE('',#2640,#2640,#2396,.T.);
#3258=EDGE_CURVE('',#2640,#2641,#1467,.T.);
#3259=EDGE_CURVE('',#2641,#2641,#2397,.T.);
#3260=EDGE_CURVE('',#2642,#2642,#2398,.T.);
#3261=EDGE_CURVE('',#2642,#2643,#1468,.T.);
#3262=EDGE_CURVE('',#2643,#2643,#2399,.T.);
#3263=EDGE_CURVE('',#2644,#2645,#1469,.T.);
#3264=EDGE_CURVE('',#2645,#2646,#99,.T.);
#3265=EDGE_CURVE('',#2646,#2647,#1470,.T.);
#3266=EDGE_CURVE('',#2647,#2644,#100,.T.);
#3267=EDGE_CURVE('',#2645,#2648,#1471,.T.);
#3268=EDGE_CURVE('',#2648,#2649,#101,.T.);
#3269=EDGE_CURVE('',#2649,#2646,#1472,.T.);
#3270=EDGE_CURVE('',#2648,#2650,#1473,.T.);
#3271=EDGE_CURVE('',#2650,#2651,#102,.T.);
#3272=EDGE_CURVE('',#2651,#2649,#1474,.T.);
#3273=EDGE_CURVE('',#2650,#2652,#1475,.T.);
#3274=EDGE_CURVE('',#2652,#2653,#103,.T.);
#3275=EDGE_CURVE('',#2653,#2651,#1476,.T.);
#3276=EDGE_CURVE('',#2654,#2653,#1477,.T.);
#3277=EDGE_CURVE('',#2652,#2655,#1478,.T.);
#3278=EDGE_CURVE('',#2655,#2654,#104,.T.);
#3279=EDGE_CURVE('',#2656,#2654,#1479,.T.);
#3280=EDGE_CURVE('',#2655,#2657,#1480,.T.);
#3281=EDGE_CURVE('',#2657,#2656,#105,.T.);
#3282=EDGE_CURVE('',#2658,#2656,#1481,.T.);
#3283=EDGE_CURVE('',#2657,#2659,#1482,.T.);
#3284=EDGE_CURVE('',#2659,#2658,#106,.T.);
#3285=EDGE_CURVE('',#2659,#2644,#1483,.T.);
#3286=EDGE_CURVE('',#2647,#2658,#1484,.T.);
#3287=EDGE_CURVE('',#2650,#2660,#1485,.T.);
#3288=EDGE_CURVE('',#2661,#2660,#1486,.T.);
#3289=EDGE_CURVE('',#2661,#2652,#1487,.T.);
#3290=EDGE_CURVE('',#2662,#2648,#1488,.T.);
#3291=EDGE_CURVE('',#2660,#2662,#1489,.T.);
#3292=EDGE_CURVE('',#2645,#2663,#1490,.T.);
#3293=EDGE_CURVE('',#2662,#2663,#1491,.T.);
#3294=EDGE_CURVE('',#2664,#2644,#1492,.T.);
#3295=EDGE_CURVE('',#2663,#2664,#1493,.T.);
#3296=EDGE_CURVE('',#2665,#2666,#1494,.T.);
#3297=EDGE_CURVE('',#2666,#2663,#107,.T.);
#3298=EDGE_CURVE('',#2665,#2664,#108,.T.);
#3299=EDGE_CURVE('',#2666,#2667,#1495,.T.);
#3300=EDGE_CURVE('',#2667,#2662,#109,.T.);
#3301=EDGE_CURVE('',#2667,#2668,#1496,.T.);
#3302=EDGE_CURVE('',#2668,#2660,#110,.T.);
#3303=EDGE_CURVE('',#2668,#2669,#1497,.T.);
#3304=EDGE_CURVE('',#2669,#2661,#111,.T.);
#3305=EDGE_CURVE('',#2670,#2661,#1498,.T.);
#3306=EDGE_CURVE('',#2669,#2671,#1499,.T.);
#3307=EDGE_CURVE('',#2671,#2670,#112,.T.);
#3308=EDGE_CURVE('',#2672,#2670,#1500,.T.);
#3309=EDGE_CURVE('',#2671,#2673,#1501,.T.);
#3310=EDGE_CURVE('',#2673,#2672,#113,.T.);
#3311=EDGE_CURVE('',#2674,#2672,#1502,.T.);
#3312=EDGE_CURVE('',#2673,#2675,#1503,.T.);
#3313=EDGE_CURVE('',#2675,#2674,#114,.T.);
#3314=EDGE_CURVE('',#2664,#2674,#1504,.T.);
#3315=EDGE_CURVE('',#2675,#2665,#1505,.T.);
#3316=EDGE_CURVE('',#2655,#2670,#1506,.T.);
#3317=EDGE_CURVE('',#2672,#2657,#1507,.T.);
#3318=EDGE_CURVE('',#2659,#2674,#1508,.T.);
#3319=EDGE_CURVE('',#2676,#2676,#2400,.T.);
#3320=EDGE_CURVE('',#2676,#2677,#1509,.T.);
#3321=EDGE_CURVE('',#2677,#2677,#2401,.T.);
#3322=EDGE_CURVE('',#2678,#2678,#2402,.T.);
#3323=EDGE_CURVE('',#2678,#2679,#1510,.T.);
#3324=EDGE_CURVE('',#2679,#2679,#2403,.T.);
#3325=EDGE_CURVE('',#2680,#2681,#1511,.T.);
#3326=EDGE_CURVE('',#2681,#2682,#1512,.T.);
#3327=EDGE_CURVE('',#2682,#2683,#1513,.T.);
#3328=EDGE_CURVE('',#2683,#2684,#1514,.T.);
#3329=EDGE_CURVE('',#2684,#2685,#1515,.T.);
#3330=EDGE_CURVE('',#2685,#2686,#1516,.T.);
#3331=EDGE_CURVE('',#2686,#2687,#1517,.T.);
#3332=EDGE_CURVE('',#2687,#2680,#1518,.T.);
#3333=EDGE_CURVE('',#2681,#2688,#1519,.T.);
#3334=EDGE_CURVE('',#2689,#2688,#1520,.T.);
#3335=EDGE_CURVE('',#2682,#2689,#1521,.T.);
#3336=EDGE_CURVE('',#2690,#2689,#1522,.T.);
#3337=EDGE_CURVE('',#2683,#2690,#1523,.T.);
#3338=EDGE_CURVE('',#2691,#2690,#1524,.T.);
#3339=EDGE_CURVE('',#2684,#2691,#1525,.T.);
#3340=EDGE_CURVE('',#2692,#2691,#1526,.T.);
#3341=EDGE_CURVE('',#2685,#2692,#1527,.T.);
#3342=EDGE_CURVE('',#2693,#2692,#1528,.T.);
#3343=EDGE_CURVE('',#2686,#2693,#1529,.T.);
#3344=EDGE_CURVE('',#2694,#2693,#1530,.T.);
#3345=EDGE_CURVE('',#2687,#2694,#1531,.T.);
#3346=EDGE_CURVE('',#2695,#2694,#1532,.T.);
#3347=EDGE_CURVE('',#2680,#2695,#1533,.T.);
#3348=EDGE_CURVE('',#2688,#2695,#1534,.T.);
#3349=EDGE_CURVE('',#2696,#2696,#2404,.T.);
#3350=EDGE_CURVE('',#2696,#2697,#1535,.T.);
#3351=EDGE_CURVE('',#2697,#2697,#2405,.T.);
#3352=EDGE_CURVE('',#2698,#2698,#2406,.T.);
#3353=EDGE_CURVE('',#2698,#2699,#1536,.T.);
#3354=EDGE_CURVE('',#2699,#2699,#2407,.T.);
#3355=EDGE_CURVE('',#2700,#2700,#2408,.T.);
#3356=EDGE_CURVE('',#2700,#2701,#1537,.T.);
#3357=EDGE_CURVE('',#2701,#2701,#2409,.T.);
#3358=EDGE_CURVE('',#2702,#2703,#1538,.T.);
#3359=EDGE_CURVE('',#2703,#2704,#115,.T.);
#3360=EDGE_CURVE('',#2704,#2705,#1539,.T.);
#3361=EDGE_CURVE('',#2705,#2702,#116,.T.);
#3362=EDGE_CURVE('',#2706,#2704,#1540,.T.);
#3363=EDGE_CURVE('',#2703,#2707,#1541,.T.);
#3364=EDGE_CURVE('',#2707,#2706,#117,.T.);
#3365=EDGE_CURVE('',#2708,#2702,#1542,.T.);
#3366=EDGE_CURVE('',#2705,#2709,#1543,.T.);
#3367=EDGE_CURVE('',#2709,#2708,#118,.T.);
#3368=EDGE_CURVE('',#2709,#2706,#1544,.T.);
#3369=EDGE_CURVE('',#2707,#2708,#1545,.T.);
#3370=EDGE_CURVE('',#2705,#2710,#1546,.T.);
#3371=EDGE_CURVE('',#2711,#2710,#2410,.T.);
#3372=EDGE_CURVE('',#2712,#2711,#1547,.T.);
#3373=EDGE_CURVE('',#2713,#2712,#2411,.T.);
#3374=EDGE_CURVE('',#2709,#2713,#1548,.T.);
#3375=EDGE_CURVE('',#2714,#2704,#1549,.T.);
#3376=EDGE_CURVE('',#2715,#2714,#1550,.T.);
#3377=EDGE_CURVE('',#2716,#2715,#1551,.T.);
#3378=EDGE_CURVE('',#2717,#2716,#1552,.T.);
#3379=EDGE_CURVE('',#2718,#2717,#1553,.T.);
#3380=EDGE_CURVE('',#2719,#2718,#1554,.T.);
#3381=EDGE_CURVE('',#2720,#2719,#1555,.T.);
#3382=EDGE_CURVE('',#2721,#2720,#1556,.T.);
#3383=EDGE_CURVE('',#2722,#2721,#1557,.T.);
#3384=EDGE_CURVE('',#2710,#2722,#1558,.T.);
#3385=EDGE_CURVE('',#2723,#2706,#1559,.T.);
#3386=EDGE_CURVE('',#2724,#2723,#2412,.T.);
#3387=EDGE_CURVE('',#2725,#2724,#1560,.T.);
#3388=EDGE_CURVE('',#2714,#2725,#2413,.T.);
#3389=EDGE_CURVE('',#2726,#2713,#1561,.T.);
#3390=EDGE_CURVE('',#2727,#2726,#1562,.T.);
#3391=EDGE_CURVE('',#2728,#2727,#1563,.T.);
#3392=EDGE_CURVE('',#2729,#2728,#1564,.T.);
#3393=EDGE_CURVE('',#2730,#2729,#1565,.T.);
#3394=EDGE_CURVE('',#2731,#2730,#1566,.T.);
#3395=EDGE_CURVE('',#2732,#2731,#1567,.T.);
#3396=EDGE_CURVE('',#2733,#2732,#1568,.T.);
#3397=EDGE_CURVE('',#2723,#2733,#1569,.T.);
#3398=EDGE_CURVE('',#2712,#2734,#1570,.T.);
#3399=EDGE_CURVE('',#2734,#2726,#119,.T.);
#3400=EDGE_CURVE('',#2735,#2733,#120,.T.);
#3401=EDGE_CURVE('',#2735,#2724,#1571,.T.);
#3402=EDGE_CURVE('',#2736,#2711,#1572,.T.);
#3403=EDGE_CURVE('',#2734,#2736,#1573,.T.);
#3404=EDGE_CURVE('',#2722,#2736,#121,.T.);
#3405=EDGE_CURVE('',#2737,#2738,#1574,.T.);
#3406=EDGE_CURVE('',#2738,#2728,#122,.T.);
#3407=EDGE_CURVE('',#2727,#2737,#123,.T.);
#3408=EDGE_CURVE('',#2738,#2739,#1575,.T.);
#3409=EDGE_CURVE('',#2739,#2729,#124,.T.);
#3410=EDGE_CURVE('',#2739,#2740,#1576,.T.);
#3411=EDGE_CURVE('',#2740,#2730,#125,.T.);
#3412=EDGE_CURVE('',#2740,#2741,#1577,.T.);
#3413=EDGE_CURVE('',#2741,#2731,#126,.T.);
#3414=EDGE_CURVE('',#2741,#2742,#1578,.T.);
#3415=EDGE_CURVE('',#2742,#2732,#127,.T.);
#3416=EDGE_CURVE('',#2742,#2735,#1579,.T.);
#3417=EDGE_CURVE('',#2734,#2737,#1580,.T.);
#3418=EDGE_CURVE('',#2740,#2743,#1581,.T.);
#3419=EDGE_CURVE('',#2744,#2743,#1582,.T.);
#3420=EDGE_CURVE('',#2744,#2741,#1583,.T.);
#3421=EDGE_CURVE('',#2745,#2739,#1584,.T.);
#3422=EDGE_CURVE('',#2743,#2745,#1585,.T.);
#3423=EDGE_CURVE('',#2738,#2746,#1586,.T.);
#3424=EDGE_CURVE('',#2745,#2746,#1587,.T.);
#3425=EDGE_CURVE('',#2747,#2737,#1588,.T.);
#3426=EDGE_CURVE('',#2746,#2747,#1589,.T.);
#3427=EDGE_CURVE('',#2720,#2746,#128,.T.);
#3428=EDGE_CURVE('',#2721,#2747,#129,.T.);
#3429=EDGE_CURVE('',#2719,#2745,#130,.T.);
#3430=EDGE_CURVE('',#2718,#2743,#131,.T.);
#3431=EDGE_CURVE('',#2717,#2744,#132,.T.);
#3432=EDGE_CURVE('',#2748,#2744,#1590,.T.);
#3433=EDGE_CURVE('',#2716,#2748,#133,.T.);
#3434=EDGE_CURVE('',#2749,#2748,#1591,.T.);
#3435=EDGE_CURVE('',#2715,#2749,#134,.T.);
#3436=EDGE_CURVE('',#2725,#2749,#1592,.T.);
#3437=EDGE_CURVE('',#2747,#2736,#1593,.T.);
#3438=EDGE_CURVE('',#2742,#2748,#1594,.T.);
#3439=EDGE_CURVE('',#2749,#2735,#1595,.T.);
#3440=EDGE_CURVE('',#2750,#2750,#2414,.T.);
#3441=EDGE_CURVE('',#2750,#2751,#1596,.T.);
#3442=EDGE_CURVE('',#2751,#2751,#2415,.T.);
#3443=EDGE_CURVE('',#2752,#2752,#2416,.T.);
#3444=EDGE_CURVE('',#2752,#2753,#1597,.T.);
#3445=EDGE_CURVE('',#2753,#2753,#2417,.T.);
#3446=EDGE_CURVE('',#2754,#2754,#2418,.T.);
#3447=EDGE_CURVE('',#2754,#2755,#1598,.T.);
#3448=EDGE_CURVE('',#2755,#2755,#2419,.T.);
#3449=EDGE_CURVE('',#2756,#2756,#2420,.T.);
#3450=EDGE_CURVE('',#2756,#2757,#1599,.T.);
#3451=EDGE_CURVE('',#2757,#2757,#2421,.T.);
#3452=EDGE_CURVE('',#2758,#2759,#1600,.T.);
#3453=EDGE_CURVE('',#2759,#2760,#135,.T.);
#3454=EDGE_CURVE('',#2760,#2761,#1601,.T.);
#3455=EDGE_CURVE('',#2758,#2761,#136,.T.);
#3456=EDGE_CURVE('',#2762,#2763,#1602,.T.);
#3457=EDGE_CURVE('',#2763,#2764,#137,.T.);
#3458=EDGE_CURVE('',#2764,#2765,#1603,.T.);
#3459=EDGE_CURVE('',#2765,#2762,#138,.T.);
#3460=EDGE_CURVE('',#2763,#2766,#1604,.T.);
#3461=EDGE_CURVE('',#2766,#2767,#139,.T.);
#3462=EDGE_CURVE('',#2767,#2764,#1605,.T.);
#3463=EDGE_CURVE('',#2768,#2769,#1606,.T.);
#3464=EDGE_CURVE('',#2769,#2770,#140,.T.);
#3465=EDGE_CURVE('',#2770,#2771,#1607,.T.);
#3466=EDGE_CURVE('',#2771,#2768,#141,.T.);
#3467=EDGE_CURVE('',#2766,#2772,#1608,.T.);
#3468=EDGE_CURVE('',#2772,#2773,#142,.T.);
#3469=EDGE_CURVE('',#2773,#2767,#1609,.T.);
#3470=EDGE_CURVE('',#2769,#2773,#1610,.T.);
#3471=EDGE_CURVE('',#2772,#2770,#1611,.T.);
#3472=EDGE_CURVE('',#2774,#2768,#1612,.T.);
#3473=EDGE_CURVE('',#2771,#2775,#1613,.T.);
#3474=EDGE_CURVE('',#2775,#2774,#143,.T.);
#3475=EDGE_CURVE('',#2776,#2774,#1614,.T.);
#3476=EDGE_CURVE('',#2775,#2777,#1615,.T.);
#3477=EDGE_CURVE('',#2777,#2776,#144,.T.);
#3478=EDGE_CURVE('',#2759,#2762,#1616,.T.);
#3479=EDGE_CURVE('',#2765,#2760,#1617,.T.);
#3480=EDGE_CURVE('',#2778,#2776,#1618,.T.);
#3481=EDGE_CURVE('',#2777,#2779,#1619,.T.);
#3482=EDGE_CURVE('',#2779,#2778,#145,.T.);
#3483=EDGE_CURVE('',#2780,#2778,#1620,.T.);
#3484=EDGE_CURVE('',#2779,#2781,#1621,.T.);
#3485=EDGE_CURVE('',#2781,#2780,#146,.T.);
#3486=EDGE_CURVE('',#2761,#2780,#1622,.T.);
#3487=EDGE_CURVE('',#2781,#2758,#1623,.T.);
#3488=EDGE_CURVE('',#2765,#2782,#1624,.T.);
#3489=EDGE_CURVE('',#2783,#2782,#1625,.T.);
#3490=EDGE_CURVE('',#2783,#2760,#1626,.T.);
#3491=EDGE_CURVE('',#2764,#2784,#1627,.T.);
#3492=EDGE_CURVE('',#2782,#2784,#1628,.T.);
#3493=EDGE_CURVE('',#2767,#2785,#1629,.T.);
#3494=EDGE_CURVE('',#2784,#2785,#1630,.T.);
#3495=EDGE_CURVE('',#2786,#2773,#1631,.T.);
#3496=EDGE_CURVE('',#2785,#2786,#1632,.T.);
#3497=EDGE_CURVE('',#2769,#2787,#1633,.T.);
#3498=EDGE_CURVE('',#2786,#2787,#1634,.T.);
#3499=EDGE_CURVE('',#2768,#2788,#1635,.T.);
#3500=EDGE_CURVE('',#2787,#2788,#1636,.T.);
#3501=EDGE_CURVE('',#2789,#2790,#1637,.T.);
#3502=EDGE_CURVE('',#2790,#2791,#147,.T.);
#3503=EDGE_CURVE('',#2791,#2792,#1638,.T.);
#3504=EDGE_CURVE('',#2789,#2792,#148,.T.);
#3505=EDGE_CURVE('',#2790,#2793,#1639,.T.);
#3506=EDGE_CURVE('',#2793,#2794,#149,.T.);
#3507=EDGE_CURVE('',#2794,#2791,#1640,.T.);
#3508=EDGE_CURVE('',#2793,#2795,#1641,.T.);
#3509=EDGE_CURVE('',#2795,#2796,#150,.T.);
#3510=EDGE_CURVE('',#2796,#2794,#1642,.T.);
#3511=EDGE_CURVE('',#2795,#2797,#1643,.T.);
#3512=EDGE_CURVE('',#2797,#2798,#151,.T.);
#3513=EDGE_CURVE('',#2798,#2796,#1644,.T.);
#3514=EDGE_CURVE('',#2797,#2799,#1645,.T.);
#3515=EDGE_CURVE('',#2799,#2788,#152,.T.);
#3516=EDGE_CURVE('',#2788,#2798,#1646,.T.);
#3517=EDGE_CURVE('',#2799,#2800,#1647,.T.);
#3518=EDGE_CURVE('',#2800,#2787,#153,.T.);
#3519=EDGE_CURVE('',#2800,#2801,#1648,.T.);
#3520=EDGE_CURVE('',#2801,#2786,#154,.T.);
#3521=EDGE_CURVE('',#2801,#2802,#1649,.T.);
#3522=EDGE_CURVE('',#2802,#2785,#155,.T.);
#3523=EDGE_CURVE('',#2802,#2803,#1650,.T.);
#3524=EDGE_CURVE('',#2803,#2784,#156,.T.);
#3525=EDGE_CURVE('',#2803,#2804,#1651,.T.);
#3526=EDGE_CURVE('',#2804,#2782,#157,.T.);
#3527=EDGE_CURVE('',#2804,#2805,#1652,.T.);
#3528=EDGE_CURVE('',#2805,#2783,#158,.T.);
#3529=EDGE_CURVE('',#2792,#2783,#1653,.T.);
#3530=EDGE_CURVE('',#2805,#2789,#1654,.T.);
#3531=EDGE_CURVE('',#2761,#2792,#1655,.T.);
#3532=EDGE_CURVE('',#2780,#2791,#1656,.T.);
#3533=EDGE_CURVE('',#2778,#2794,#1657,.T.);
#3534=EDGE_CURVE('',#2776,#2796,#1658,.T.);
#3535=EDGE_CURVE('',#2774,#2798,#1659,.T.);
#3536=EDGE_CURVE('',#2806,#2806,#2422,.T.);
#3537=EDGE_CURVE('',#2806,#2807,#1660,.T.);
#3538=EDGE_CURVE('',#2807,#2807,#2423,.T.);
#3539=EDGE_CURVE('',#2808,#2808,#2424,.T.);
#3540=EDGE_CURVE('',#2808,#2809,#1661,.T.);
#3541=EDGE_CURVE('',#2809,#2809,#2425,.T.);
#3542=EDGE_CURVE('',#2810,#2810,#2426,.T.);
#3543=EDGE_CURVE('',#2810,#2811,#1662,.T.);
#3544=EDGE_CURVE('',#2811,#2811,#2427,.T.);
#3545=EDGE_CURVE('',#2812,#2812,#2428,.T.);
#3546=EDGE_CURVE('',#2812,#2813,#1663,.T.);
#3547=EDGE_CURVE('',#2813,#2813,#2429,.T.);
#3548=EDGE_CURVE('',#2814,#2815,#1664,.T.);
#3549=EDGE_CURVE('',#2815,#2816,#159,.T.);
#3550=EDGE_CURVE('',#2816,#2817,#1665,.T.);
#3551=EDGE_CURVE('',#2814,#2817,#160,.T.);
#3552=EDGE_CURVE('',#2818,#2819,#1666,.T.);
#3553=EDGE_CURVE('',#2819,#2820,#161,.T.);
#3554=EDGE_CURVE('',#2820,#2821,#1667,.T.);
#3555=EDGE_CURVE('',#2821,#2818,#162,.T.);
#3556=EDGE_CURVE('',#2819,#2822,#1668,.T.);
#3557=EDGE_CURVE('',#2822,#2823,#163,.T.);
#3558=EDGE_CURVE('',#2823,#2820,#1669,.T.);
#3559=EDGE_CURVE('',#2824,#2825,#1670,.T.);
#3560=EDGE_CURVE('',#2825,#2826,#164,.T.);
#3561=EDGE_CURVE('',#2826,#2827,#1671,.T.);
#3562=EDGE_CURVE('',#2827,#2824,#165,.T.);
#3563=EDGE_CURVE('',#2822,#2828,#1672,.T.);
#3564=EDGE_CURVE('',#2828,#2829,#166,.T.);
#3565=EDGE_CURVE('',#2829,#2823,#1673,.T.);
#3566=EDGE_CURVE('',#2825,#2829,#1674,.T.);
#3567=EDGE_CURVE('',#2828,#2826,#1675,.T.);
#3568=EDGE_CURVE('',#2830,#2824,#1676,.T.);
#3569=EDGE_CURVE('',#2827,#2831,#1677,.T.);
#3570=EDGE_CURVE('',#2831,#2830,#167,.T.);
#3571=EDGE_CURVE('',#2832,#2830,#1678,.T.);
#3572=EDGE_CURVE('',#2831,#2833,#1679,.T.);
#3573=EDGE_CURVE('',#2833,#2832,#168,.T.);
#3574=EDGE_CURVE('',#2815,#2818,#1680,.T.);
#3575=EDGE_CURVE('',#2821,#2816,#1681,.T.);
#3576=EDGE_CURVE('',#2834,#2832,#1682,.T.);
#3577=EDGE_CURVE('',#2833,#2835,#1683,.T.);
#3578=EDGE_CURVE('',#2835,#2834,#169,.T.);
#3579=EDGE_CURVE('',#2836,#2834,#1684,.T.);
#3580=EDGE_CURVE('',#2835,#2837,#1685,.T.);
#3581=EDGE_CURVE('',#2837,#2836,#170,.T.);
#3582=EDGE_CURVE('',#2817,#2836,#1686,.T.);
#3583=EDGE_CURVE('',#2837,#2814,#1687,.T.);
#3584=EDGE_CURVE('',#2821,#2838,#1688,.T.);
#3585=EDGE_CURVE('',#2839,#2838,#1689,.T.);
#3586=EDGE_CURVE('',#2839,#2816,#1690,.T.);
#3587=EDGE_CURVE('',#2820,#2840,#1691,.T.);
#3588=EDGE_CURVE('',#2838,#2840,#1692,.T.);
#3589=EDGE_CURVE('',#2823,#2841,#1693,.T.);
#3590=EDGE_CURVE('',#2840,#2841,#1694,.T.);
#3591=EDGE_CURVE('',#2842,#2829,#1695,.T.);
#3592=EDGE_CURVE('',#2841,#2842,#1696,.T.);
#3593=EDGE_CURVE('',#2825,#2843,#1697,.T.);
#3594=EDGE_CURVE('',#2842,#2843,#1698,.T.);
#3595=EDGE_CURVE('',#2824,#2844,#1699,.T.);
#3596=EDGE_CURVE('',#2843,#2844,#1700,.T.);
#3597=EDGE_CURVE('',#2845,#2846,#1701,.T.);
#3598=EDGE_CURVE('',#2846,#2847,#171,.T.);
#3599=EDGE_CURVE('',#2847,#2848,#1702,.T.);
#3600=EDGE_CURVE('',#2845,#2848,#172,.T.);
#3601=EDGE_CURVE('',#2846,#2849,#1703,.T.);
#3602=EDGE_CURVE('',#2849,#2850,#173,.T.);
#3603=EDGE_CURVE('',#2850,#2847,#1704,.T.);
#3604=EDGE_CURVE('',#2849,#2851,#1705,.T.);
#3605=EDGE_CURVE('',#2851,#2852,#174,.T.);
#3606=EDGE_CURVE('',#2852,#2850,#1706,.T.);
#3607=EDGE_CURVE('',#2851,#2853,#1707,.T.);
#3608=EDGE_CURVE('',#2853,#2854,#175,.T.);
#3609=EDGE_CURVE('',#2854,#2852,#1708,.T.);
#3610=EDGE_CURVE('',#2853,#2855,#1709,.T.);
#3611=EDGE_CURVE('',#2855,#2844,#176,.T.);
#3612=EDGE_CURVE('',#2844,#2854,#1710,.T.);
#3613=EDGE_CURVE('',#2855,#2856,#1711,.T.);
#3614=EDGE_CURVE('',#2856,#2843,#177,.T.);
#3615=EDGE_CURVE('',#2856,#2857,#1712,.T.);
#3616=EDGE_CURVE('',#2857,#2842,#178,.T.);
#3617=EDGE_CURVE('',#2857,#2858,#1713,.T.);
#3618=EDGE_CURVE('',#2858,#2841,#179,.T.);
#3619=EDGE_CURVE('',#2858,#2859,#1714,.T.);
#3620=EDGE_CURVE('',#2859,#2840,#180,.T.);
#3621=EDGE_CURVE('',#2859,#2860,#1715,.T.);
#3622=EDGE_CURVE('',#2860,#2838,#181,.T.);
#3623=EDGE_CURVE('',#2860,#2861,#1716,.T.);
#3624=EDGE_CURVE('',#2861,#2839,#182,.T.);
#3625=EDGE_CURVE('',#2848,#2839,#1717,.T.);
#3626=EDGE_CURVE('',#2861,#2845,#1718,.T.);
#3627=EDGE_CURVE('',#2817,#2848,#1719,.T.);
#3628=EDGE_CURVE('',#2836,#2847,#1720,.T.);
#3629=EDGE_CURVE('',#2834,#2850,#1721,.T.);
#3630=EDGE_CURVE('',#2832,#2852,#1722,.T.);
#3631=EDGE_CURVE('',#2830,#2854,#1723,.T.);
#3632=EDGE_CURVE('',#2862,#2863,#1724,.T.);
#3633=EDGE_CURVE('',#2863,#2864,#183,.T.);
#3634=EDGE_CURVE('',#2864,#2865,#1725,.T.);
#3635=EDGE_CURVE('',#2865,#2862,#184,.T.);
#3636=EDGE_CURVE('',#2866,#2867,#1726,.T.);
#3637=EDGE_CURVE('',#2867,#2868,#185,.T.);
#3638=EDGE_CURVE('',#2868,#2869,#1727,.T.);
#3639=EDGE_CURVE('',#2869,#2866,#186,.T.);
#3640=EDGE_CURVE('',#2867,#2870,#1728,.T.);
#3641=EDGE_CURVE('',#2870,#2871,#187,.T.);
#3642=EDGE_CURVE('',#2871,#2868,#1729,.T.);
#3643=EDGE_CURVE('',#2870,#2872,#1730,.T.);
#3644=EDGE_CURVE('',#2872,#2873,#188,.T.);
#3645=EDGE_CURVE('',#2873,#2871,#1731,.T.);
#3646=EDGE_CURVE('',#2872,#2874,#1732,.T.);
#3647=EDGE_CURVE('',#2874,#2875,#189,.T.);
#3648=EDGE_CURVE('',#2875,#2873,#1733,.T.);
#3649=EDGE_CURVE('',#2874,#2876,#1734,.T.);
#3650=EDGE_CURVE('',#2876,#2877,#190,.T.);
#3651=EDGE_CURVE('',#2877,#2875,#1735,.T.);
#3652=EDGE_CURVE('',#2878,#2877,#1736,.T.);
#3653=EDGE_CURVE('',#2876,#2879,#1737,.T.);
#3654=EDGE_CURVE('',#2879,#2878,#191,.T.);
#3655=EDGE_CURVE('',#2880,#2878,#1738,.T.);
#3656=EDGE_CURVE('',#2879,#2881,#1739,.T.);
#3657=EDGE_CURVE('',#2881,#2880,#192,.T.);
#3658=EDGE_CURVE('',#2882,#2880,#1740,.T.);
#3659=EDGE_CURVE('',#2881,#2883,#1741,.T.);
#3660=EDGE_CURVE('',#2883,#2882,#193,.T.);
#3661=EDGE_CURVE('',#2884,#2882,#1742,.T.);
#3662=EDGE_CURVE('',#2883,#2885,#1743,.T.);
#3663=EDGE_CURVE('',#2885,#2884,#194,.T.);
#3664=EDGE_CURVE('',#2863,#2884,#1744,.T.);
#3665=EDGE_CURVE('',#2885,#2864,#1745,.T.);
#3666=EDGE_CURVE('',#2869,#2862,#1746,.T.);
#3667=EDGE_CURVE('',#2865,#2866,#1747,.T.);
#3668=EDGE_CURVE('',#2882,#2886,#1748,.T.);
#3669=EDGE_CURVE('',#2887,#2886,#1749,.T.);
#3670=EDGE_CURVE('',#2887,#2880,#1750,.T.);
#3671=EDGE_CURVE('',#2888,#2884,#1751,.T.);
#3672=EDGE_CURVE('',#2886,#2888,#1752,.T.);
#3673=EDGE_CURVE('',#2863,#2889,#1753,.T.);
#3674=EDGE_CURVE('',#2888,#2889,#1754,.T.);
#3675=EDGE_CURVE('',#2890,#2862,#1755,.T.);
#3676=EDGE_CURVE('',#2889,#2890,#1756,.T.);
#3677=EDGE_CURVE('',#2869,#2891,#1757,.T.);
#3678=EDGE_CURVE('',#2890,#2891,#1758,.T.);
#3679=EDGE_CURVE('',#2892,#2868,#1759,.T.);
#3680=EDGE_CURVE('',#2891,#2892,#1760,.T.);
#3681=EDGE_CURVE('',#2893,#2894,#1761,.T.);
#3682=EDGE_CURVE('',#2894,#2889,#195,.T.);
#3683=EDGE_CURVE('',#2893,#2890,#196,.T.);
#3684=EDGE_CURVE('',#2894,#2895,#1762,.T.);
#3685=EDGE_CURVE('',#2895,#2888,#197,.T.);
#3686=EDGE_CURVE('',#2895,#2896,#1763,.T.);
#3687=EDGE_CURVE('',#2896,#2886,#198,.T.);
#3688=EDGE_CURVE('',#2896,#2897,#1764,.T.);
#3689=EDGE_CURVE('',#2897,#2887,#199,.T.);
#3690=EDGE_CURVE('',#2897,#2898,#1765,.T.);
#3691=EDGE_CURVE('',#2898,#2899,#200,.T.);
#3692=EDGE_CURVE('',#2899,#2887,#1766,.T.);
#3693=EDGE_CURVE('',#2900,#2899,#1767,.T.);
#3694=EDGE_CURVE('',#2898,#2901,#1768,.T.);
#3695=EDGE_CURVE('',#2901,#2900,#201,.T.);
#3696=EDGE_CURVE('',#2902,#2900,#1769,.T.);
#3697=EDGE_CURVE('',#2901,#2903,#1770,.T.);
#3698=EDGE_CURVE('',#2903,#2902,#202,.T.);
#3699=EDGE_CURVE('',#2904,#2902,#1771,.T.);
#3700=EDGE_CURVE('',#2903,#2905,#1772,.T.);
#3701=EDGE_CURVE('',#2905,#2904,#203,.T.);
#3702=EDGE_CURVE('',#2906,#2904,#1773,.T.);
#3703=EDGE_CURVE('',#2905,#2907,#1774,.T.);
#3704=EDGE_CURVE('',#2907,#2906,#204,.T.);
#3705=EDGE_CURVE('',#2892,#2906,#1775,.T.);
#3706=EDGE_CURVE('',#2907,#2908,#1776,.T.);
#3707=EDGE_CURVE('',#2908,#2892,#205,.T.);
#3708=EDGE_CURVE('',#2908,#2909,#1777,.T.);
#3709=EDGE_CURVE('',#2909,#2891,#206,.T.);
#3710=EDGE_CURVE('',#2909,#2893,#1778,.T.);
#3711=EDGE_CURVE('',#2875,#2902,#1779,.T.);
#3712=EDGE_CURVE('',#2904,#2873,#1780,.T.);
#3713=EDGE_CURVE('',#2871,#2906,#1781,.T.);
#3714=EDGE_CURVE('',#2878,#2899,#1782,.T.);
#3715=EDGE_CURVE('',#2900,#2877,#1783,.T.);
#3716=ORIENTED_EDGE('',*,*,#2910,.F.);
#3717=ORIENTED_EDGE('',*,*,#2911,.T.);
#3718=ORIENTED_EDGE('',*,*,#2912,.F.);
#3719=ORIENTED_EDGE('',*,*,#2911,.F.);
#3720=ORIENTED_EDGE('',*,*,#2913,.F.);
#3721=ORIENTED_EDGE('',*,*,#2914,.T.);
#3722=ORIENTED_EDGE('',*,*,#2915,.F.);
#3723=ORIENTED_EDGE('',*,*,#2914,.F.);
#3724=ORIENTED_EDGE('',*,*,#2916,.F.);
#3725=ORIENTED_EDGE('',*,*,#2917,.T.);
#3726=ORIENTED_EDGE('',*,*,#2918,.F.);
#3727=ORIENTED_EDGE('',*,*,#2917,.F.);
#3728=ORIENTED_EDGE('',*,*,#2919,.F.);
#3729=ORIENTED_EDGE('',*,*,#2920,.T.);
#3730=ORIENTED_EDGE('',*,*,#2921,.F.);
#3731=ORIENTED_EDGE('',*,*,#2920,.F.);
#3732=ORIENTED_EDGE('',*,*,#2922,.F.);
#3733=ORIENTED_EDGE('',*,*,#2923,.T.);
#3734=ORIENTED_EDGE('',*,*,#2924,.F.);
#3735=ORIENTED_EDGE('',*,*,#2923,.F.);
#3736=ORIENTED_EDGE('',*,*,#2925,.F.);
#3737=ORIENTED_EDGE('',*,*,#2926,.T.);
#3738=ORIENTED_EDGE('',*,*,#2927,.F.);
#3739=ORIENTED_EDGE('',*,*,#2926,.F.);
#3740=ORIENTED_EDGE('',*,*,#2928,.F.);
#3741=ORIENTED_EDGE('',*,*,#2929,.T.);
#3742=ORIENTED_EDGE('',*,*,#2930,.F.);
#3743=ORIENTED_EDGE('',*,*,#2929,.F.);
#3744=ORIENTED_EDGE('',*,*,#2931,.F.);
#3745=ORIENTED_EDGE('',*,*,#2932,.T.);
#3746=ORIENTED_EDGE('',*,*,#2933,.F.);
#3747=ORIENTED_EDGE('',*,*,#2932,.F.);
#3748=ORIENTED_EDGE('',*,*,#2934,.T.);
#3749=ORIENTED_EDGE('',*,*,#2935,.T.);
#3750=ORIENTED_EDGE('',*,*,#2936,.T.);
#3751=ORIENTED_EDGE('',*,*,#2937,.T.);
#3752=ORIENTED_EDGE('',*,*,#2937,.F.);
#3753=ORIENTED_EDGE('',*,*,#2938,.F.);
#3754=ORIENTED_EDGE('',*,*,#2939,.F.);
#3755=ORIENTED_EDGE('',*,*,#2940,.F.);
#3756=ORIENTED_EDGE('',*,*,#2936,.F.);
#3757=ORIENTED_EDGE('',*,*,#2941,.T.);
#3758=ORIENTED_EDGE('',*,*,#2942,.F.);
#3759=ORIENTED_EDGE('',*,*,#2943,.T.);
#3760=ORIENTED_EDGE('',*,*,#2944,.F.);
#3761=ORIENTED_EDGE('',*,*,#2945,.T.);
#3762=ORIENTED_EDGE('',*,*,#2946,.F.);
#3763=ORIENTED_EDGE('',*,*,#2938,.T.);
#3764=ORIENTED_EDGE('',*,*,#2933,.T.);
#3765=ORIENTED_EDGE('',*,*,#2930,.T.);
#3766=ORIENTED_EDGE('',*,*,#2927,.T.);
#3767=ORIENTED_EDGE('',*,*,#2924,.T.);
#3768=ORIENTED_EDGE('',*,*,#2921,.T.);
#3769=ORIENTED_EDGE('',*,*,#2918,.T.);
#3770=ORIENTED_EDGE('',*,*,#2915,.T.);
#3771=ORIENTED_EDGE('',*,*,#2912,.T.);
#3772=ORIENTED_EDGE('',*,*,#2947,.T.);
#3773=ORIENTED_EDGE('',*,*,#2948,.T.);
#3774=ORIENTED_EDGE('',*,*,#2942,.T.);
#3775=ORIENTED_EDGE('',*,*,#2949,.T.);
#3776=ORIENTED_EDGE('',*,*,#2948,.F.);
#3777=ORIENTED_EDGE('',*,*,#2950,.F.);
#3778=ORIENTED_EDGE('',*,*,#2951,.F.);
#3779=ORIENTED_EDGE('',*,*,#2943,.F.);
#3780=ORIENTED_EDGE('',*,*,#2952,.T.);
#3781=ORIENTED_EDGE('',*,*,#2953,.T.);
#3782=ORIENTED_EDGE('',*,*,#2944,.T.);
#3783=ORIENTED_EDGE('',*,*,#2951,.T.);
#3784=ORIENTED_EDGE('',*,*,#2954,.T.);
#3785=ORIENTED_EDGE('',*,*,#2939,.T.);
#3786=ORIENTED_EDGE('',*,*,#2946,.T.);
#3787=ORIENTED_EDGE('',*,*,#2955,.T.);
#3788=ORIENTED_EDGE('',*,*,#2953,.F.);
#3789=ORIENTED_EDGE('',*,*,#2956,.F.);
#3790=ORIENTED_EDGE('',*,*,#2955,.F.);
#3791=ORIENTED_EDGE('',*,*,#2945,.F.);
#3792=ORIENTED_EDGE('',*,*,#2935,.F.);
#3793=ORIENTED_EDGE('',*,*,#2957,.F.);
#3794=ORIENTED_EDGE('',*,*,#2949,.F.);
#3795=ORIENTED_EDGE('',*,*,#2941,.F.);
#3796=ORIENTED_EDGE('',*,*,#2934,.F.);
#3797=ORIENTED_EDGE('',*,*,#2940,.T.);
#3798=ORIENTED_EDGE('',*,*,#2954,.F.);
#3799=ORIENTED_EDGE('',*,*,#2956,.T.);
#3800=ORIENTED_EDGE('',*,*,#2952,.F.);
#3801=ORIENTED_EDGE('',*,*,#2950,.T.);
#3802=ORIENTED_EDGE('',*,*,#2947,.F.);
#3803=ORIENTED_EDGE('',*,*,#2957,.T.);
#3804=ORIENTED_EDGE('',*,*,#2931,.T.);
#3805=ORIENTED_EDGE('',*,*,#2928,.T.);
#3806=ORIENTED_EDGE('',*,*,#2925,.T.);
#3807=ORIENTED_EDGE('',*,*,#2922,.T.);
#3808=ORIENTED_EDGE('',*,*,#2919,.T.);
#3809=ORIENTED_EDGE('',*,*,#2916,.T.);
#3810=ORIENTED_EDGE('',*,*,#2913,.T.);
#3811=ORIENTED_EDGE('',*,*,#2910,.T.);
#3812=ORIENTED_EDGE('',*,*,#2958,.F.);
#3813=ORIENTED_EDGE('',*,*,#2959,.T.);
#3814=ORIENTED_EDGE('',*,*,#2960,.F.);
#3815=ORIENTED_EDGE('',*,*,#2959,.F.);
#3816=ORIENTED_EDGE('',*,*,#2961,.T.);
#3817=ORIENTED_EDGE('',*,*,#2962,.T.);
#3818=ORIENTED_EDGE('',*,*,#2963,.T.);
#3819=ORIENTED_EDGE('',*,*,#2964,.F.);
#3820=ORIENTED_EDGE('',*,*,#2965,.T.);
#3821=ORIENTED_EDGE('',*,*,#2966,.T.);
#3822=ORIENTED_EDGE('',*,*,#2967,.T.);
#3823=ORIENTED_EDGE('',*,*,#2962,.F.);
#3824=ORIENTED_EDGE('',*,*,#2968,.T.);
#3825=ORIENTED_EDGE('',*,*,#2969,.T.);
#3826=ORIENTED_EDGE('',*,*,#2970,.T.);
#3827=ORIENTED_EDGE('',*,*,#2966,.F.);
#3828=ORIENTED_EDGE('',*,*,#2971,.T.);
#3829=ORIENTED_EDGE('',*,*,#2972,.T.);
#3830=ORIENTED_EDGE('',*,*,#2973,.T.);
#3831=ORIENTED_EDGE('',*,*,#2969,.F.);
#3832=ORIENTED_EDGE('',*,*,#2974,.T.);
#3833=ORIENTED_EDGE('',*,*,#2975,.T.);
#3834=ORIENTED_EDGE('',*,*,#2976,.T.);
#3835=ORIENTED_EDGE('',*,*,#2972,.F.);
#3836=ORIENTED_EDGE('',*,*,#2977,.T.);
#3837=ORIENTED_EDGE('',*,*,#2975,.F.);
#3838=ORIENTED_EDGE('',*,*,#2978,.T.);
#3839=ORIENTED_EDGE('',*,*,#2979,.T.);
#3840=ORIENTED_EDGE('',*,*,#2980,.T.);
#3841=ORIENTED_EDGE('',*,*,#2979,.F.);
#3842=ORIENTED_EDGE('',*,*,#2981,.T.);
#3843=ORIENTED_EDGE('',*,*,#2982,.T.);
#3844=ORIENTED_EDGE('',*,*,#2983,.T.);
#3845=ORIENTED_EDGE('',*,*,#2982,.F.);
#3846=ORIENTED_EDGE('',*,*,#2984,.T.);
#3847=ORIENTED_EDGE('',*,*,#2985,.T.);
#3848=ORIENTED_EDGE('',*,*,#2986,.T.);
#3849=ORIENTED_EDGE('',*,*,#2985,.F.);
#3850=ORIENTED_EDGE('',*,*,#2987,.T.);
#3851=ORIENTED_EDGE('',*,*,#2988,.T.);
#3852=ORIENTED_EDGE('',*,*,#2989,.T.);
#3853=ORIENTED_EDGE('',*,*,#2988,.F.);
#3854=ORIENTED_EDGE('',*,*,#2990,.T.);
#3855=ORIENTED_EDGE('',*,*,#2991,.T.);
#3856=ORIENTED_EDGE('',*,*,#2992,.T.);
#3857=ORIENTED_EDGE('',*,*,#2991,.F.);
#3858=ORIENTED_EDGE('',*,*,#2993,.T.);
#3859=ORIENTED_EDGE('',*,*,#2994,.T.);
#3860=ORIENTED_EDGE('',*,*,#2995,.T.);
#3861=ORIENTED_EDGE('',*,*,#2994,.F.);
#3862=ORIENTED_EDGE('',*,*,#2996,.T.);
#3863=ORIENTED_EDGE('',*,*,#2964,.T.);
#3864=ORIENTED_EDGE('',*,*,#2983,.F.);
#3865=ORIENTED_EDGE('',*,*,#2997,.T.);
#3866=ORIENTED_EDGE('',*,*,#2998,.T.);
#3867=ORIENTED_EDGE('',*,*,#2999,.T.);
#3868=ORIENTED_EDGE('',*,*,#2986,.F.);
#3869=ORIENTED_EDGE('',*,*,#3000,.F.);
#3870=ORIENTED_EDGE('',*,*,#3001,.T.);
#3871=ORIENTED_EDGE('',*,*,#2997,.F.);
#3872=ORIENTED_EDGE('',*,*,#2989,.F.);
#3873=ORIENTED_EDGE('',*,*,#3002,.T.);
#3874=ORIENTED_EDGE('',*,*,#3003,.T.);
#3875=ORIENTED_EDGE('',*,*,#3000,.T.);
#3876=ORIENTED_EDGE('',*,*,#2992,.F.);
#3877=ORIENTED_EDGE('',*,*,#3004,.F.);
#3878=ORIENTED_EDGE('',*,*,#3005,.T.);
#3879=ORIENTED_EDGE('',*,*,#3002,.F.);
#3880=ORIENTED_EDGE('',*,*,#2995,.F.);
#3881=ORIENTED_EDGE('',*,*,#3006,.T.);
#3882=ORIENTED_EDGE('',*,*,#3007,.T.);
#3883=ORIENTED_EDGE('',*,*,#3004,.T.);
#3884=ORIENTED_EDGE('',*,*,#2963,.F.);
#3885=ORIENTED_EDGE('',*,*,#3008,.F.);
#3886=ORIENTED_EDGE('',*,*,#3009,.T.);
#3887=ORIENTED_EDGE('',*,*,#3006,.F.);
#3888=ORIENTED_EDGE('',*,*,#2961,.F.);
#3889=ORIENTED_EDGE('',*,*,#2996,.F.);
#3890=ORIENTED_EDGE('',*,*,#2993,.F.);
#3891=ORIENTED_EDGE('',*,*,#2990,.F.);
#3892=ORIENTED_EDGE('',*,*,#2987,.F.);
#3893=ORIENTED_EDGE('',*,*,#2984,.F.);
#3894=ORIENTED_EDGE('',*,*,#2981,.F.);
#3895=ORIENTED_EDGE('',*,*,#2978,.F.);
#3896=ORIENTED_EDGE('',*,*,#2974,.F.);
#3897=ORIENTED_EDGE('',*,*,#2971,.F.);
#3898=ORIENTED_EDGE('',*,*,#2968,.F.);
#3899=ORIENTED_EDGE('',*,*,#2965,.F.);
#3900=ORIENTED_EDGE('',*,*,#2958,.T.);
#3901=ORIENTED_EDGE('',*,*,#2977,.F.);
#3902=ORIENTED_EDGE('',*,*,#3010,.T.);
#3903=ORIENTED_EDGE('',*,*,#3011,.T.);
#3904=ORIENTED_EDGE('',*,*,#3012,.T.);
#3905=ORIENTED_EDGE('',*,*,#2976,.F.);
#3906=ORIENTED_EDGE('',*,*,#3012,.F.);
#3907=ORIENTED_EDGE('',*,*,#3013,.T.);
#3908=ORIENTED_EDGE('',*,*,#3014,.F.);
#3909=ORIENTED_EDGE('',*,*,#3011,.F.);
#3910=ORIENTED_EDGE('',*,*,#3015,.F.);
#3911=ORIENTED_EDGE('',*,*,#2998,.F.);
#3912=ORIENTED_EDGE('',*,*,#3001,.F.);
#3913=ORIENTED_EDGE('',*,*,#3003,.F.);
#3914=ORIENTED_EDGE('',*,*,#3005,.F.);
#3915=ORIENTED_EDGE('',*,*,#3007,.F.);
#3916=ORIENTED_EDGE('',*,*,#3009,.F.);
#3917=ORIENTED_EDGE('',*,*,#3016,.F.);
#3918=ORIENTED_EDGE('',*,*,#3017,.F.);
#3919=ORIENTED_EDGE('',*,*,#3018,.F.);
#3920=ORIENTED_EDGE('',*,*,#3013,.F.);
#3921=ORIENTED_EDGE('',*,*,#2960,.T.);
#3922=ORIENTED_EDGE('',*,*,#2973,.F.);
#3923=ORIENTED_EDGE('',*,*,#3014,.T.);
#3924=ORIENTED_EDGE('',*,*,#3018,.T.);
#3925=ORIENTED_EDGE('',*,*,#3019,.T.);
#3926=ORIENTED_EDGE('',*,*,#2970,.F.);
#3927=ORIENTED_EDGE('',*,*,#3019,.F.);
#3928=ORIENTED_EDGE('',*,*,#3017,.T.);
#3929=ORIENTED_EDGE('',*,*,#3020,.F.);
#3930=ORIENTED_EDGE('',*,*,#2967,.F.);
#3931=ORIENTED_EDGE('',*,*,#3020,.T.);
#3932=ORIENTED_EDGE('',*,*,#3016,.T.);
#3933=ORIENTED_EDGE('',*,*,#3008,.T.);
#3934=ORIENTED_EDGE('',*,*,#2980,.F.);
#3935=ORIENTED_EDGE('',*,*,#2999,.F.);
#3936=ORIENTED_EDGE('',*,*,#3015,.T.);
#3937=ORIENTED_EDGE('',*,*,#3010,.F.);
#3938=ORIENTED_EDGE('',*,*,#3021,.T.);
#3939=ORIENTED_EDGE('',*,*,#3022,.T.);
#3940=ORIENTED_EDGE('',*,*,#3023,.T.);
#3941=ORIENTED_EDGE('',*,*,#3024,.T.);
#3942=ORIENTED_EDGE('',*,*,#3025,.T.);
#3943=ORIENTED_EDGE('',*,*,#3026,.T.);
#3944=ORIENTED_EDGE('',*,*,#3021,.F.);
#3945=ORIENTED_EDGE('',*,*,#3027,.T.);
#3946=ORIENTED_EDGE('',*,*,#3028,.T.);
#3947=ORIENTED_EDGE('',*,*,#3029,.T.);
#3948=ORIENTED_EDGE('',*,*,#3025,.F.);
#3949=ORIENTED_EDGE('',*,*,#3030,.T.);
#3950=ORIENTED_EDGE('',*,*,#3030,.F.);
#3951=ORIENTED_EDGE('',*,*,#3027,.F.);
#3952=ORIENTED_EDGE('',*,*,#3024,.F.);
#3953=ORIENTED_EDGE('',*,*,#3031,.T.);
#3954=ORIENTED_EDGE('',*,*,#3032,.T.);
#3955=ORIENTED_EDGE('',*,*,#3033,.T.);
#3956=ORIENTED_EDGE('',*,*,#3034,.T.);
#3957=ORIENTED_EDGE('',*,*,#3035,.T.);
#3958=ORIENTED_EDGE('',*,*,#3036,.T.);
#3959=ORIENTED_EDGE('',*,*,#3037,.T.);
#3960=ORIENTED_EDGE('',*,*,#3038,.T.);
#3961=ORIENTED_EDGE('',*,*,#3039,.T.);
#3962=ORIENTED_EDGE('',*,*,#3034,.F.);
#3963=ORIENTED_EDGE('',*,*,#3040,.T.);
#3964=ORIENTED_EDGE('',*,*,#3041,.T.);
#3965=ORIENTED_EDGE('',*,*,#3042,.T.);
#3966=ORIENTED_EDGE('',*,*,#3038,.F.);
#3967=ORIENTED_EDGE('',*,*,#3043,.T.);
#3968=ORIENTED_EDGE('',*,*,#3043,.F.);
#3969=ORIENTED_EDGE('',*,*,#3040,.F.);
#3970=ORIENTED_EDGE('',*,*,#3037,.F.);
#3971=ORIENTED_EDGE('',*,*,#3044,.T.);
#3972=ORIENTED_EDGE('',*,*,#3045,.T.);
#3973=ORIENTED_EDGE('',*,*,#3046,.T.);
#3974=ORIENTED_EDGE('',*,*,#3047,.F.);
#3975=ORIENTED_EDGE('',*,*,#3048,.T.);
#3976=ORIENTED_EDGE('',*,*,#3049,.F.);
#3977=ORIENTED_EDGE('',*,*,#3048,.F.);
#3978=ORIENTED_EDGE('',*,*,#3050,.F.);
#3979=ORIENTED_EDGE('',*,*,#3051,.T.);
#3980=ORIENTED_EDGE('',*,*,#3052,.F.);
#3981=ORIENTED_EDGE('',*,*,#3051,.F.);
#3982=ORIENTED_EDGE('',*,*,#3053,.F.);
#3983=ORIENTED_EDGE('',*,*,#3054,.T.);
#3984=ORIENTED_EDGE('',*,*,#3055,.F.);
#3985=ORIENTED_EDGE('',*,*,#3054,.F.);
#3986=ORIENTED_EDGE('',*,*,#3056,.F.);
#3987=ORIENTED_EDGE('',*,*,#3057,.T.);
#3988=ORIENTED_EDGE('',*,*,#3058,.F.);
#3989=ORIENTED_EDGE('',*,*,#3057,.F.);
#3990=ORIENTED_EDGE('',*,*,#3059,.T.);
#3991=ORIENTED_EDGE('',*,*,#3045,.F.);
#3992=ORIENTED_EDGE('',*,*,#3060,.F.);
#3993=ORIENTED_EDGE('',*,*,#3032,.F.);
#3994=ORIENTED_EDGE('',*,*,#3029,.F.);
#3995=ORIENTED_EDGE('',*,*,#3061,.T.);
#3996=ORIENTED_EDGE('',*,*,#3062,.F.);
#3997=ORIENTED_EDGE('',*,*,#3063,.T.);
#3998=ORIENTED_EDGE('',*,*,#3035,.F.);
#3999=ORIENTED_EDGE('',*,*,#3064,.T.);
#4000=ORIENTED_EDGE('',*,*,#3065,.T.);
#4001=ORIENTED_EDGE('',*,*,#3066,.T.);
#4002=ORIENTED_EDGE('',*,*,#3026,.F.);
#4003=ORIENTED_EDGE('',*,*,#3063,.F.);
#4004=ORIENTED_EDGE('',*,*,#3067,.F.);
#4005=ORIENTED_EDGE('',*,*,#3068,.F.);
#4006=ORIENTED_EDGE('',*,*,#3069,.F.);
#4007=ORIENTED_EDGE('',*,*,#3070,.F.);
#4008=ORIENTED_EDGE('',*,*,#3047,.T.);
#4009=ORIENTED_EDGE('',*,*,#3053,.T.);
#4010=ORIENTED_EDGE('',*,*,#3039,.F.);
#4011=ORIENTED_EDGE('',*,*,#3071,.F.);
#4012=ORIENTED_EDGE('',*,*,#3072,.F.);
#4013=ORIENTED_EDGE('',*,*,#3073,.F.);
#4014=ORIENTED_EDGE('',*,*,#3074,.F.);
#4015=ORIENTED_EDGE('',*,*,#3075,.F.);
#4016=ORIENTED_EDGE('',*,*,#3076,.F.);
#4017=ORIENTED_EDGE('',*,*,#3077,.F.);
#4018=ORIENTED_EDGE('',*,*,#3078,.F.);
#4019=ORIENTED_EDGE('',*,*,#3064,.F.);
#4020=ORIENTED_EDGE('',*,*,#3050,.T.);
#4021=ORIENTED_EDGE('',*,*,#3056,.T.);
#4022=ORIENTED_EDGE('',*,*,#3022,.F.);
#4023=ORIENTED_EDGE('',*,*,#3070,.T.);
#4024=ORIENTED_EDGE('',*,*,#3079,.T.);
#4025=ORIENTED_EDGE('',*,*,#3080,.T.);
#4026=ORIENTED_EDGE('',*,*,#3042,.F.);
#4027=ORIENTED_EDGE('',*,*,#3081,.T.);
#4028=ORIENTED_EDGE('',*,*,#3082,.F.);
#4029=ORIENTED_EDGE('',*,*,#3071,.T.);
#4030=ORIENTED_EDGE('',*,*,#3083,.T.);
#4031=ORIENTED_EDGE('',*,*,#3084,.T.);
#4032=ORIENTED_EDGE('',*,*,#3085,.T.);
#4033=ORIENTED_EDGE('',*,*,#3086,.F.);
#4034=ORIENTED_EDGE('',*,*,#3087,.T.);
#4035=ORIENTED_EDGE('',*,*,#3088,.T.);
#4036=ORIENTED_EDGE('',*,*,#3089,.T.);
#4037=ORIENTED_EDGE('',*,*,#3090,.T.);
#4038=ORIENTED_EDGE('',*,*,#3091,.T.);
#4039=ORIENTED_EDGE('',*,*,#3092,.T.);
#4040=ORIENTED_EDGE('',*,*,#3093,.T.);
#4041=ORIENTED_EDGE('',*,*,#3088,.F.);
#4042=ORIENTED_EDGE('',*,*,#3094,.T.);
#4043=ORIENTED_EDGE('',*,*,#3095,.T.);
#4044=ORIENTED_EDGE('',*,*,#3096,.T.);
#4045=ORIENTED_EDGE('',*,*,#3097,.T.);
#4046=ORIENTED_EDGE('',*,*,#3098,.T.);
#4047=ORIENTED_EDGE('',*,*,#3099,.T.);
#4048=ORIENTED_EDGE('',*,*,#3100,.T.);
#4049=ORIENTED_EDGE('',*,*,#3092,.F.);
#4050=ORIENTED_EDGE('',*,*,#3101,.T.);
#4051=ORIENTED_EDGE('',*,*,#3099,.F.);
#4052=ORIENTED_EDGE('',*,*,#3102,.T.);
#4053=ORIENTED_EDGE('',*,*,#3095,.F.);
#4054=ORIENTED_EDGE('',*,*,#3103,.T.);
#4055=ORIENTED_EDGE('',*,*,#3097,.F.);
#4056=ORIENTED_EDGE('',*,*,#3104,.T.);
#4057=ORIENTED_EDGE('',*,*,#3105,.T.);
#4058=ORIENTED_EDGE('',*,*,#3106,.T.);
#4059=ORIENTED_EDGE('',*,*,#3105,.F.);
#4060=ORIENTED_EDGE('',*,*,#3107,.T.);
#4061=ORIENTED_EDGE('',*,*,#3108,.T.);
#4062=ORIENTED_EDGE('',*,*,#3109,.T.);
#4063=ORIENTED_EDGE('',*,*,#3090,.F.);
#4064=ORIENTED_EDGE('',*,*,#3110,.T.);
#4065=ORIENTED_EDGE('',*,*,#3084,.F.);
#4066=ORIENTED_EDGE('',*,*,#3111,.T.);
#4067=ORIENTED_EDGE('',*,*,#3108,.F.);
#4068=ORIENTED_EDGE('',*,*,#3112,.T.);
#4069=ORIENTED_EDGE('',*,*,#3113,.T.);
#4070=ORIENTED_EDGE('',*,*,#3114,.T.);
#4071=ORIENTED_EDGE('',*,*,#3113,.F.);
#4072=ORIENTED_EDGE('',*,*,#3115,.T.);
#4073=ORIENTED_EDGE('',*,*,#3116,.T.);
#4074=ORIENTED_EDGE('',*,*,#3117,.T.);
#4075=ORIENTED_EDGE('',*,*,#3116,.F.);
#4076=ORIENTED_EDGE('',*,*,#3118,.T.);
#4077=ORIENTED_EDGE('',*,*,#3086,.T.);
#4078=ORIENTED_EDGE('',*,*,#3110,.F.);
#4079=ORIENTED_EDGE('',*,*,#3119,.T.);
#4080=ORIENTED_EDGE('',*,*,#3120,.F.);
#4081=ORIENTED_EDGE('',*,*,#3121,.T.);
#4082=ORIENTED_EDGE('',*,*,#3089,.F.);
#4083=ORIENTED_EDGE('',*,*,#3122,.T.);
#4084=ORIENTED_EDGE('',*,*,#3123,.F.);
#4085=ORIENTED_EDGE('',*,*,#3119,.F.);
#4086=ORIENTED_EDGE('',*,*,#3093,.F.);
#4087=ORIENTED_EDGE('',*,*,#3124,.T.);
#4088=ORIENTED_EDGE('',*,*,#3125,.F.);
#4089=ORIENTED_EDGE('',*,*,#3122,.F.);
#4090=ORIENTED_EDGE('',*,*,#3100,.F.);
#4091=ORIENTED_EDGE('',*,*,#3126,.F.);
#4092=ORIENTED_EDGE('',*,*,#3127,.F.);
#4093=ORIENTED_EDGE('',*,*,#3124,.F.);
#4094=ORIENTED_EDGE('',*,*,#3101,.F.);
#4095=ORIENTED_EDGE('',*,*,#3128,.T.);
#4096=ORIENTED_EDGE('',*,*,#3129,.F.);
#4097=ORIENTED_EDGE('',*,*,#3126,.T.);
#4098=ORIENTED_EDGE('',*,*,#3094,.F.);
#4099=ORIENTED_EDGE('',*,*,#3130,.T.);
#4100=ORIENTED_EDGE('',*,*,#3131,.F.);
#4101=ORIENTED_EDGE('',*,*,#3128,.F.);
#4102=ORIENTED_EDGE('',*,*,#3096,.F.);
#4103=ORIENTED_EDGE('',*,*,#3102,.F.);
#4104=ORIENTED_EDGE('',*,*,#3098,.F.);
#4105=ORIENTED_EDGE('',*,*,#3091,.F.);
#4106=ORIENTED_EDGE('',*,*,#3087,.F.);
#4107=ORIENTED_EDGE('',*,*,#3109,.F.);
#4108=ORIENTED_EDGE('',*,*,#3083,.F.);
#4109=ORIENTED_EDGE('',*,*,#3118,.F.);
#4110=ORIENTED_EDGE('',*,*,#3115,.F.);
#4111=ORIENTED_EDGE('',*,*,#3112,.F.);
#4112=ORIENTED_EDGE('',*,*,#3107,.F.);
#4113=ORIENTED_EDGE('',*,*,#3104,.F.);
#4114=ORIENTED_EDGE('',*,*,#3049,.T.);
#4115=ORIENTED_EDGE('',*,*,#3052,.T.);
#4116=ORIENTED_EDGE('',*,*,#3055,.T.);
#4117=ORIENTED_EDGE('',*,*,#3058,.T.);
#4118=ORIENTED_EDGE('',*,*,#3069,.T.);
#4119=ORIENTED_EDGE('',*,*,#3132,.T.);
#4120=ORIENTED_EDGE('',*,*,#3133,.T.);
#4121=ORIENTED_EDGE('',*,*,#3079,.F.);
#4122=ORIENTED_EDGE('',*,*,#3068,.T.);
#4123=ORIENTED_EDGE('',*,*,#3134,.T.);
#4124=ORIENTED_EDGE('',*,*,#3135,.T.);
#4125=ORIENTED_EDGE('',*,*,#3132,.F.);
#4126=ORIENTED_EDGE('',*,*,#3067,.T.);
#4127=ORIENTED_EDGE('',*,*,#3062,.T.);
#4128=ORIENTED_EDGE('',*,*,#3136,.T.);
#4129=ORIENTED_EDGE('',*,*,#3134,.F.);
#4130=ORIENTED_EDGE('',*,*,#3078,.T.);
#4131=ORIENTED_EDGE('',*,*,#3137,.T.);
#4132=ORIENTED_EDGE('',*,*,#3138,.T.);
#4133=ORIENTED_EDGE('',*,*,#3065,.F.);
#4134=ORIENTED_EDGE('',*,*,#3077,.T.);
#4135=ORIENTED_EDGE('',*,*,#3139,.T.);
#4136=ORIENTED_EDGE('',*,*,#3131,.T.);
#4137=ORIENTED_EDGE('',*,*,#3137,.F.);
#4138=ORIENTED_EDGE('',*,*,#3129,.T.);
#4139=ORIENTED_EDGE('',*,*,#3139,.F.);
#4140=ORIENTED_EDGE('',*,*,#3076,.T.);
#4141=ORIENTED_EDGE('',*,*,#3140,.T.);
#4142=ORIENTED_EDGE('',*,*,#3127,.T.);
#4143=ORIENTED_EDGE('',*,*,#3140,.F.);
#4144=ORIENTED_EDGE('',*,*,#3075,.T.);
#4145=ORIENTED_EDGE('',*,*,#3141,.T.);
#4146=ORIENTED_EDGE('',*,*,#3125,.T.);
#4147=ORIENTED_EDGE('',*,*,#3141,.F.);
#4148=ORIENTED_EDGE('',*,*,#3074,.T.);
#4149=ORIENTED_EDGE('',*,*,#3142,.T.);
#4150=ORIENTED_EDGE('',*,*,#3123,.T.);
#4151=ORIENTED_EDGE('',*,*,#3142,.F.);
#4152=ORIENTED_EDGE('',*,*,#3073,.T.);
#4153=ORIENTED_EDGE('',*,*,#3143,.T.);
#4154=ORIENTED_EDGE('',*,*,#3120,.T.);
#4155=ORIENTED_EDGE('',*,*,#3143,.F.);
#4156=ORIENTED_EDGE('',*,*,#3072,.T.);
#4157=ORIENTED_EDGE('',*,*,#3082,.T.);
#4158=ORIENTED_EDGE('',*,*,#3085,.F.);
#4159=ORIENTED_EDGE('',*,*,#3121,.F.);
#4160=ORIENTED_EDGE('',*,*,#3081,.F.);
#4161=ORIENTED_EDGE('',*,*,#3041,.F.);
#4162=ORIENTED_EDGE('',*,*,#3046,.F.);
#4163=ORIENTED_EDGE('',*,*,#3059,.F.);
#4164=ORIENTED_EDGE('',*,*,#3031,.F.);
#4165=ORIENTED_EDGE('',*,*,#3023,.F.);
#4166=ORIENTED_EDGE('',*,*,#3080,.F.);
#4167=ORIENTED_EDGE('',*,*,#3144,.F.);
#4168=ORIENTED_EDGE('',*,*,#3117,.F.);
#4169=ORIENTED_EDGE('',*,*,#3144,.T.);
#4170=ORIENTED_EDGE('',*,*,#3133,.F.);
#4171=ORIENTED_EDGE('',*,*,#3145,.F.);
#4172=ORIENTED_EDGE('',*,*,#3114,.F.);
#4173=ORIENTED_EDGE('',*,*,#3145,.T.);
#4174=ORIENTED_EDGE('',*,*,#3135,.F.);
#4175=ORIENTED_EDGE('',*,*,#3146,.F.);
#4176=ORIENTED_EDGE('',*,*,#3111,.F.);
#4177=ORIENTED_EDGE('',*,*,#3146,.T.);
#4178=ORIENTED_EDGE('',*,*,#3136,.F.);
#4179=ORIENTED_EDGE('',*,*,#3147,.F.);
#4180=ORIENTED_EDGE('',*,*,#3106,.F.);
#4181=ORIENTED_EDGE('',*,*,#3147,.T.);
#4182=ORIENTED_EDGE('',*,*,#3061,.F.);
#4183=ORIENTED_EDGE('',*,*,#3028,.F.);
#4184=ORIENTED_EDGE('',*,*,#3033,.F.);
#4185=ORIENTED_EDGE('',*,*,#3060,.T.);
#4186=ORIENTED_EDGE('',*,*,#3044,.F.);
#4187=ORIENTED_EDGE('',*,*,#3036,.F.);
#4188=ORIENTED_EDGE('',*,*,#3066,.F.);
#4189=ORIENTED_EDGE('',*,*,#3148,.F.);
#4190=ORIENTED_EDGE('',*,*,#3103,.F.);
#4191=ORIENTED_EDGE('',*,*,#3148,.T.);
#4192=ORIENTED_EDGE('',*,*,#3138,.F.);
#4193=ORIENTED_EDGE('',*,*,#3130,.F.);
#4194=ORIENTED_EDGE('',*,*,#3149,.T.);
#4195=ORIENTED_EDGE('',*,*,#3150,.T.);
#4196=ORIENTED_EDGE('',*,*,#3151,.T.);
#4197=ORIENTED_EDGE('',*,*,#3152,.T.);
#4198=ORIENTED_EDGE('',*,*,#3153,.T.);
#4199=ORIENTED_EDGE('',*,*,#3154,.T.);
#4200=ORIENTED_EDGE('',*,*,#3155,.T.);
#4201=ORIENTED_EDGE('',*,*,#3156,.T.);
#4202=ORIENTED_EDGE('',*,*,#3157,.T.);
#4203=ORIENTED_EDGE('',*,*,#3158,.T.);
#4204=ORIENTED_EDGE('',*,*,#3159,.T.);
#4205=ORIENTED_EDGE('',*,*,#3154,.F.);
#4206=ORIENTED_EDGE('',*,*,#3160,.T.);
#4207=ORIENTED_EDGE('',*,*,#3161,.T.);
#4208=ORIENTED_EDGE('',*,*,#3162,.T.);
#4209=ORIENTED_EDGE('',*,*,#3158,.F.);
#4210=ORIENTED_EDGE('',*,*,#3163,.T.);
#4211=ORIENTED_EDGE('',*,*,#3164,.T.);
#4212=ORIENTED_EDGE('',*,*,#3165,.T.);
#4213=ORIENTED_EDGE('',*,*,#3161,.F.);
#4214=ORIENTED_EDGE('',*,*,#3166,.T.);
#4215=ORIENTED_EDGE('',*,*,#3167,.T.);
#4216=ORIENTED_EDGE('',*,*,#3168,.T.);
#4217=ORIENTED_EDGE('',*,*,#3164,.F.);
#4218=ORIENTED_EDGE('',*,*,#3169,.T.);
#4219=ORIENTED_EDGE('',*,*,#3167,.F.);
#4220=ORIENTED_EDGE('',*,*,#3170,.T.);
#4221=ORIENTED_EDGE('',*,*,#3171,.T.);
#4222=ORIENTED_EDGE('',*,*,#3172,.T.);
#4223=ORIENTED_EDGE('',*,*,#3171,.F.);
#4224=ORIENTED_EDGE('',*,*,#3173,.T.);
#4225=ORIENTED_EDGE('',*,*,#3174,.T.);
#4226=ORIENTED_EDGE('',*,*,#3175,.T.);
#4227=ORIENTED_EDGE('',*,*,#3174,.F.);
#4228=ORIENTED_EDGE('',*,*,#3176,.T.);
#4229=ORIENTED_EDGE('',*,*,#3177,.T.);
#4230=ORIENTED_EDGE('',*,*,#3178,.T.);
#4231=ORIENTED_EDGE('',*,*,#3177,.F.);
#4232=ORIENTED_EDGE('',*,*,#3179,.T.);
#4233=ORIENTED_EDGE('',*,*,#3180,.T.);
#4234=ORIENTED_EDGE('',*,*,#3181,.T.);
#4235=ORIENTED_EDGE('',*,*,#3180,.F.);
#4236=ORIENTED_EDGE('',*,*,#3182,.T.);
#4237=ORIENTED_EDGE('',*,*,#3150,.F.);
#4238=ORIENTED_EDGE('',*,*,#3183,.T.);
#4239=ORIENTED_EDGE('',*,*,#3152,.F.);
#4240=ORIENTED_EDGE('',*,*,#3184,.T.);
#4241=ORIENTED_EDGE('',*,*,#3156,.F.);
#4242=ORIENTED_EDGE('',*,*,#3175,.F.);
#4243=ORIENTED_EDGE('',*,*,#3185,.T.);
#4244=ORIENTED_EDGE('',*,*,#3186,.F.);
#4245=ORIENTED_EDGE('',*,*,#3187,.T.);
#4246=ORIENTED_EDGE('',*,*,#3178,.F.);
#4247=ORIENTED_EDGE('',*,*,#3188,.F.);
#4248=ORIENTED_EDGE('',*,*,#3189,.F.);
#4249=ORIENTED_EDGE('',*,*,#3185,.F.);
#4250=ORIENTED_EDGE('',*,*,#3181,.F.);
#4251=ORIENTED_EDGE('',*,*,#3190,.T.);
#4252=ORIENTED_EDGE('',*,*,#3191,.F.);
#4253=ORIENTED_EDGE('',*,*,#3188,.T.);
#4254=ORIENTED_EDGE('',*,*,#3149,.F.);
#4255=ORIENTED_EDGE('',*,*,#3192,.F.);
#4256=ORIENTED_EDGE('',*,*,#3193,.F.);
#4257=ORIENTED_EDGE('',*,*,#3190,.F.);
#4258=ORIENTED_EDGE('',*,*,#3183,.F.);
#4259=ORIENTED_EDGE('',*,*,#3194,.T.);
#4260=ORIENTED_EDGE('',*,*,#3195,.F.);
#4261=ORIENTED_EDGE('',*,*,#3192,.T.);
#4262=ORIENTED_EDGE('',*,*,#3155,.F.);
#4263=ORIENTED_EDGE('',*,*,#3196,.F.);
#4264=ORIENTED_EDGE('',*,*,#3197,.F.);
#4265=ORIENTED_EDGE('',*,*,#3194,.F.);
#4266=ORIENTED_EDGE('',*,*,#3153,.F.);
#4267=ORIENTED_EDGE('',*,*,#3184,.F.);
#4268=ORIENTED_EDGE('',*,*,#3151,.F.);
#4269=ORIENTED_EDGE('',*,*,#3182,.F.);
#4270=ORIENTED_EDGE('',*,*,#3179,.F.);
#4271=ORIENTED_EDGE('',*,*,#3176,.F.);
#4272=ORIENTED_EDGE('',*,*,#3173,.F.);
#4273=ORIENTED_EDGE('',*,*,#3170,.F.);
#4274=ORIENTED_EDGE('',*,*,#3166,.F.);
#4275=ORIENTED_EDGE('',*,*,#3163,.F.);
#4276=ORIENTED_EDGE('',*,*,#3160,.F.);
#4277=ORIENTED_EDGE('',*,*,#3157,.F.);
#4278=ORIENTED_EDGE('',*,*,#3198,.T.);
#4279=ORIENTED_EDGE('',*,*,#3199,.T.);
#4280=ORIENTED_EDGE('',*,*,#3193,.T.);
#4281=ORIENTED_EDGE('',*,*,#3200,.F.);
#4282=ORIENTED_EDGE('',*,*,#3201,.T.);
#4283=ORIENTED_EDGE('',*,*,#3202,.T.);
#4284=ORIENTED_EDGE('',*,*,#3191,.T.);
#4285=ORIENTED_EDGE('',*,*,#3199,.F.);
#4286=ORIENTED_EDGE('',*,*,#3203,.T.);
#4287=ORIENTED_EDGE('',*,*,#3204,.T.);
#4288=ORIENTED_EDGE('',*,*,#3189,.T.);
#4289=ORIENTED_EDGE('',*,*,#3202,.F.);
#4290=ORIENTED_EDGE('',*,*,#3205,.T.);
#4291=ORIENTED_EDGE('',*,*,#3206,.T.);
#4292=ORIENTED_EDGE('',*,*,#3186,.T.);
#4293=ORIENTED_EDGE('',*,*,#3204,.F.);
#4294=ORIENTED_EDGE('',*,*,#3207,.T.);
#4295=ORIENTED_EDGE('',*,*,#3208,.T.);
#4296=ORIENTED_EDGE('',*,*,#3209,.T.);
#4297=ORIENTED_EDGE('',*,*,#3206,.F.);
#4298=ORIENTED_EDGE('',*,*,#3210,.T.);
#4299=ORIENTED_EDGE('',*,*,#3208,.F.);
#4300=ORIENTED_EDGE('',*,*,#3211,.T.);
#4301=ORIENTED_EDGE('',*,*,#3212,.T.);
#4302=ORIENTED_EDGE('',*,*,#3213,.T.);
#4303=ORIENTED_EDGE('',*,*,#3212,.F.);
#4304=ORIENTED_EDGE('',*,*,#3214,.T.);
#4305=ORIENTED_EDGE('',*,*,#3215,.T.);
#4306=ORIENTED_EDGE('',*,*,#3216,.T.);
#4307=ORIENTED_EDGE('',*,*,#3215,.F.);
#4308=ORIENTED_EDGE('',*,*,#3217,.T.);
#4309=ORIENTED_EDGE('',*,*,#3218,.T.);
#4310=ORIENTED_EDGE('',*,*,#3219,.T.);
#4311=ORIENTED_EDGE('',*,*,#3218,.F.);
#4312=ORIENTED_EDGE('',*,*,#3220,.T.);
#4313=ORIENTED_EDGE('',*,*,#3221,.T.);
#4314=ORIENTED_EDGE('',*,*,#3222,.T.);
#4315=ORIENTED_EDGE('',*,*,#3221,.F.);
#4316=ORIENTED_EDGE('',*,*,#3223,.T.);
#4317=ORIENTED_EDGE('',*,*,#3224,.T.);
#4318=ORIENTED_EDGE('',*,*,#3197,.T.);
#4319=ORIENTED_EDGE('',*,*,#3224,.F.);
#4320=ORIENTED_EDGE('',*,*,#3225,.T.);
#4321=ORIENTED_EDGE('',*,*,#3226,.T.);
#4322=ORIENTED_EDGE('',*,*,#3195,.T.);
#4323=ORIENTED_EDGE('',*,*,#3226,.F.);
#4324=ORIENTED_EDGE('',*,*,#3227,.T.);
#4325=ORIENTED_EDGE('',*,*,#3200,.T.);
#4326=ORIENTED_EDGE('',*,*,#3165,.F.);
#4327=ORIENTED_EDGE('',*,*,#3228,.T.);
#4328=ORIENTED_EDGE('',*,*,#3216,.F.);
#4329=ORIENTED_EDGE('',*,*,#3229,.T.);
#4330=ORIENTED_EDGE('',*,*,#3162,.F.);
#4331=ORIENTED_EDGE('',*,*,#3229,.F.);
#4332=ORIENTED_EDGE('',*,*,#3219,.F.);
#4333=ORIENTED_EDGE('',*,*,#3230,.F.);
#4334=ORIENTED_EDGE('',*,*,#3159,.F.);
#4335=ORIENTED_EDGE('',*,*,#3230,.T.);
#4336=ORIENTED_EDGE('',*,*,#3222,.F.);
#4337=ORIENTED_EDGE('',*,*,#3196,.T.);
#4338=ORIENTED_EDGE('',*,*,#3198,.F.);
#4339=ORIENTED_EDGE('',*,*,#3227,.F.);
#4340=ORIENTED_EDGE('',*,*,#3225,.F.);
#4341=ORIENTED_EDGE('',*,*,#3223,.F.);
#4342=ORIENTED_EDGE('',*,*,#3220,.F.);
#4343=ORIENTED_EDGE('',*,*,#3217,.F.);
#4344=ORIENTED_EDGE('',*,*,#3214,.F.);
#4345=ORIENTED_EDGE('',*,*,#3211,.F.);
#4346=ORIENTED_EDGE('',*,*,#3207,.F.);
#4347=ORIENTED_EDGE('',*,*,#3205,.F.);
#4348=ORIENTED_EDGE('',*,*,#3203,.F.);
#4349=ORIENTED_EDGE('',*,*,#3201,.F.);
#4350=ORIENTED_EDGE('',*,*,#3169,.F.);
#4351=ORIENTED_EDGE('',*,*,#3231,.T.);
#4352=ORIENTED_EDGE('',*,*,#3210,.F.);
#4353=ORIENTED_EDGE('',*,*,#3232,.T.);
#4354=ORIENTED_EDGE('',*,*,#3168,.F.);
#4355=ORIENTED_EDGE('',*,*,#3232,.F.);
#4356=ORIENTED_EDGE('',*,*,#3213,.F.);
#4357=ORIENTED_EDGE('',*,*,#3228,.F.);
#4358=ORIENTED_EDGE('',*,*,#3172,.F.);
#4359=ORIENTED_EDGE('',*,*,#3187,.F.);
#4360=ORIENTED_EDGE('',*,*,#3209,.F.);
#4361=ORIENTED_EDGE('',*,*,#3231,.F.);
#4362=ORIENTED_EDGE('',*,*,#3233,.F.);
#4363=ORIENTED_EDGE('',*,*,#3234,.T.);
#4364=ORIENTED_EDGE('',*,*,#3235,.F.);
#4365=ORIENTED_EDGE('',*,*,#3234,.F.);
#4366=ORIENTED_EDGE('',*,*,#3236,.F.);
#4367=ORIENTED_EDGE('',*,*,#3237,.T.);
#4368=ORIENTED_EDGE('',*,*,#3238,.F.);
#4369=ORIENTED_EDGE('',*,*,#3237,.F.);
#4370=ORIENTED_EDGE('',*,*,#3239,.F.);
#4371=ORIENTED_EDGE('',*,*,#3240,.T.);
#4372=ORIENTED_EDGE('',*,*,#3241,.F.);
#4373=ORIENTED_EDGE('',*,*,#3240,.F.);
#4374=ORIENTED_EDGE('',*,*,#3242,.F.);
#4375=ORIENTED_EDGE('',*,*,#3243,.T.);
#4376=ORIENTED_EDGE('',*,*,#3244,.F.);
#4377=ORIENTED_EDGE('',*,*,#3243,.F.);
#4378=ORIENTED_EDGE('',*,*,#3245,.F.);
#4379=ORIENTED_EDGE('',*,*,#3246,.T.);
#4380=ORIENTED_EDGE('',*,*,#3247,.F.);
#4381=ORIENTED_EDGE('',*,*,#3246,.F.);
#4382=ORIENTED_EDGE('',*,*,#3248,.F.);
#4383=ORIENTED_EDGE('',*,*,#3249,.T.);
#4384=ORIENTED_EDGE('',*,*,#3250,.F.);
#4385=ORIENTED_EDGE('',*,*,#3249,.F.);
#4386=ORIENTED_EDGE('',*,*,#3251,.F.);
#4387=ORIENTED_EDGE('',*,*,#3252,.T.);
#4388=ORIENTED_EDGE('',*,*,#3253,.F.);
#4389=ORIENTED_EDGE('',*,*,#3252,.F.);
#4390=ORIENTED_EDGE('',*,*,#3254,.F.);
#4391=ORIENTED_EDGE('',*,*,#3255,.T.);
#4392=ORIENTED_EDGE('',*,*,#3256,.F.);
#4393=ORIENTED_EDGE('',*,*,#3255,.F.);
#4394=ORIENTED_EDGE('',*,*,#3257,.F.);
#4395=ORIENTED_EDGE('',*,*,#3258,.T.);
#4396=ORIENTED_EDGE('',*,*,#3259,.F.);
#4397=ORIENTED_EDGE('',*,*,#3258,.F.);
#4398=ORIENTED_EDGE('',*,*,#3260,.F.);
#4399=ORIENTED_EDGE('',*,*,#3261,.T.);
#4400=ORIENTED_EDGE('',*,*,#3262,.F.);
#4401=ORIENTED_EDGE('',*,*,#3261,.F.);
#4402=ORIENTED_EDGE('',*,*,#3263,.T.);
#4403=ORIENTED_EDGE('',*,*,#3264,.T.);
#4404=ORIENTED_EDGE('',*,*,#3265,.T.);
#4405=ORIENTED_EDGE('',*,*,#3266,.T.);
#4406=ORIENTED_EDGE('',*,*,#3267,.T.);
#4407=ORIENTED_EDGE('',*,*,#3268,.T.);
#4408=ORIENTED_EDGE('',*,*,#3269,.T.);
#4409=ORIENTED_EDGE('',*,*,#3264,.F.);
#4410=ORIENTED_EDGE('',*,*,#3270,.T.);
#4411=ORIENTED_EDGE('',*,*,#3271,.T.);
#4412=ORIENTED_EDGE('',*,*,#3272,.T.);
#4413=ORIENTED_EDGE('',*,*,#3268,.F.);
#4414=ORIENTED_EDGE('',*,*,#3273,.T.);
#4415=ORIENTED_EDGE('',*,*,#3274,.T.);
#4416=ORIENTED_EDGE('',*,*,#3275,.T.);
#4417=ORIENTED_EDGE('',*,*,#3271,.F.);
#4418=ORIENTED_EDGE('',*,*,#3276,.T.);
#4419=ORIENTED_EDGE('',*,*,#3274,.F.);
#4420=ORIENTED_EDGE('',*,*,#3277,.T.);
#4421=ORIENTED_EDGE('',*,*,#3278,.T.);
#4422=ORIENTED_EDGE('',*,*,#3279,.T.);
#4423=ORIENTED_EDGE('',*,*,#3278,.F.);
#4424=ORIENTED_EDGE('',*,*,#3280,.T.);
#4425=ORIENTED_EDGE('',*,*,#3281,.T.);
#4426=ORIENTED_EDGE('',*,*,#3282,.T.);
#4427=ORIENTED_EDGE('',*,*,#3281,.F.);
#4428=ORIENTED_EDGE('',*,*,#3283,.T.);
#4429=ORIENTED_EDGE('',*,*,#3284,.T.);
#4430=ORIENTED_EDGE('',*,*,#3285,.T.);
#4431=ORIENTED_EDGE('',*,*,#3266,.F.);
#4432=ORIENTED_EDGE('',*,*,#3286,.T.);
#4433=ORIENTED_EDGE('',*,*,#3284,.F.);
#4434=ORIENTED_EDGE('',*,*,#3273,.F.);
#4435=ORIENTED_EDGE('',*,*,#3287,.T.);
#4436=ORIENTED_EDGE('',*,*,#3288,.F.);
#4437=ORIENTED_EDGE('',*,*,#3289,.T.);
#4438=ORIENTED_EDGE('',*,*,#3270,.F.);
#4439=ORIENTED_EDGE('',*,*,#3290,.F.);
#4440=ORIENTED_EDGE('',*,*,#3291,.F.);
#4441=ORIENTED_EDGE('',*,*,#3287,.F.);
#4442=ORIENTED_EDGE('',*,*,#3267,.F.);
#4443=ORIENTED_EDGE('',*,*,#3292,.T.);
#4444=ORIENTED_EDGE('',*,*,#3293,.F.);
#4445=ORIENTED_EDGE('',*,*,#3290,.T.);
#4446=ORIENTED_EDGE('',*,*,#3263,.F.);
#4447=ORIENTED_EDGE('',*,*,#3294,.F.);
#4448=ORIENTED_EDGE('',*,*,#3295,.F.);
#4449=ORIENTED_EDGE('',*,*,#3292,.F.);
#4450=ORIENTED_EDGE('',*,*,#3265,.F.);
#4451=ORIENTED_EDGE('',*,*,#3269,.F.);
#4452=ORIENTED_EDGE('',*,*,#3272,.F.);
#4453=ORIENTED_EDGE('',*,*,#3275,.F.);
#4454=ORIENTED_EDGE('',*,*,#3276,.F.);
#4455=ORIENTED_EDGE('',*,*,#3279,.F.);
#4456=ORIENTED_EDGE('',*,*,#3282,.F.);
#4457=ORIENTED_EDGE('',*,*,#3286,.F.);
#4458=ORIENTED_EDGE('',*,*,#3241,.T.);
#4459=ORIENTED_EDGE('',*,*,#3244,.T.);
#4460=ORIENTED_EDGE('',*,*,#3247,.T.);
#4461=ORIENTED_EDGE('',*,*,#3250,.T.);
#4462=ORIENTED_EDGE('',*,*,#3253,.T.);
#4463=ORIENTED_EDGE('',*,*,#3256,.T.);
#4464=ORIENTED_EDGE('',*,*,#3259,.T.);
#4465=ORIENTED_EDGE('',*,*,#3262,.T.);
#4466=ORIENTED_EDGE('',*,*,#3238,.T.);
#4467=ORIENTED_EDGE('',*,*,#3235,.T.);
#4468=ORIENTED_EDGE('',*,*,#3296,.T.);
#4469=ORIENTED_EDGE('',*,*,#3297,.T.);
#4470=ORIENTED_EDGE('',*,*,#3295,.T.);
#4471=ORIENTED_EDGE('',*,*,#3298,.F.);
#4472=ORIENTED_EDGE('',*,*,#3299,.T.);
#4473=ORIENTED_EDGE('',*,*,#3300,.T.);
#4474=ORIENTED_EDGE('',*,*,#3293,.T.);
#4475=ORIENTED_EDGE('',*,*,#3297,.F.);
#4476=ORIENTED_EDGE('',*,*,#3301,.T.);
#4477=ORIENTED_EDGE('',*,*,#3302,.T.);
#4478=ORIENTED_EDGE('',*,*,#3291,.T.);
#4479=ORIENTED_EDGE('',*,*,#3300,.F.);
#4480=ORIENTED_EDGE('',*,*,#3288,.T.);
#4481=ORIENTED_EDGE('',*,*,#3302,.F.);
#4482=ORIENTED_EDGE('',*,*,#3303,.T.);
#4483=ORIENTED_EDGE('',*,*,#3304,.T.);
#4484=ORIENTED_EDGE('',*,*,#3305,.T.);
#4485=ORIENTED_EDGE('',*,*,#3304,.F.);
#4486=ORIENTED_EDGE('',*,*,#3306,.T.);
#4487=ORIENTED_EDGE('',*,*,#3307,.T.);
#4488=ORIENTED_EDGE('',*,*,#3308,.T.);
#4489=ORIENTED_EDGE('',*,*,#3307,.F.);
#4490=ORIENTED_EDGE('',*,*,#3309,.T.);
#4491=ORIENTED_EDGE('',*,*,#3310,.T.);
#4492=ORIENTED_EDGE('',*,*,#3311,.T.);
#4493=ORIENTED_EDGE('',*,*,#3310,.F.);
#4494=ORIENTED_EDGE('',*,*,#3312,.T.);
#4495=ORIENTED_EDGE('',*,*,#3313,.T.);
#4496=ORIENTED_EDGE('',*,*,#3314,.T.);
#4497=ORIENTED_EDGE('',*,*,#3313,.F.);
#4498=ORIENTED_EDGE('',*,*,#3315,.T.);
#4499=ORIENTED_EDGE('',*,*,#3298,.T.);
#4500=ORIENTED_EDGE('',*,*,#3280,.F.);
#4501=ORIENTED_EDGE('',*,*,#3316,.T.);
#4502=ORIENTED_EDGE('',*,*,#3308,.F.);
#4503=ORIENTED_EDGE('',*,*,#3317,.T.);
#4504=ORIENTED_EDGE('',*,*,#3283,.F.);
#4505=ORIENTED_EDGE('',*,*,#3317,.F.);
#4506=ORIENTED_EDGE('',*,*,#3311,.F.);
#4507=ORIENTED_EDGE('',*,*,#3318,.F.);
#4508=ORIENTED_EDGE('',*,*,#3285,.F.);
#4509=ORIENTED_EDGE('',*,*,#3318,.T.);
#4510=ORIENTED_EDGE('',*,*,#3314,.F.);
#4511=ORIENTED_EDGE('',*,*,#3294,.T.);
#4512=ORIENTED_EDGE('',*,*,#3296,.F.);
#4513=ORIENTED_EDGE('',*,*,#3315,.F.);
#4514=ORIENTED_EDGE('',*,*,#3312,.F.);
#4515=ORIENTED_EDGE('',*,*,#3309,.F.);
#4516=ORIENTED_EDGE('',*,*,#3306,.F.);
#4517=ORIENTED_EDGE('',*,*,#3303,.F.);
#4518=ORIENTED_EDGE('',*,*,#3301,.F.);
#4519=ORIENTED_EDGE('',*,*,#3299,.F.);
#4520=ORIENTED_EDGE('',*,*,#3239,.T.);
#4521=ORIENTED_EDGE('',*,*,#3242,.T.);
#4522=ORIENTED_EDGE('',*,*,#3245,.T.);
#4523=ORIENTED_EDGE('',*,*,#3248,.T.);
#4524=ORIENTED_EDGE('',*,*,#3251,.T.);
#4525=ORIENTED_EDGE('',*,*,#3254,.T.);
#4526=ORIENTED_EDGE('',*,*,#3257,.T.);
#4527=ORIENTED_EDGE('',*,*,#3260,.T.);
#4528=ORIENTED_EDGE('',*,*,#3236,.T.);
#4529=ORIENTED_EDGE('',*,*,#3233,.T.);
#4530=ORIENTED_EDGE('',*,*,#3277,.F.);
#4531=ORIENTED_EDGE('',*,*,#3289,.F.);
#4532=ORIENTED_EDGE('',*,*,#3305,.F.);
#4533=ORIENTED_EDGE('',*,*,#3316,.F.);
#4534=ORIENTED_EDGE('',*,*,#3319,.F.);
#4535=ORIENTED_EDGE('',*,*,#3320,.T.);
#4536=ORIENTED_EDGE('',*,*,#3321,.F.);
#4537=ORIENTED_EDGE('',*,*,#3320,.F.);
#4538=ORIENTED_EDGE('',*,*,#3322,.F.);
#4539=ORIENTED_EDGE('',*,*,#3323,.T.);
#4540=ORIENTED_EDGE('',*,*,#3324,.F.);
#4541=ORIENTED_EDGE('',*,*,#3323,.F.);
#4542=ORIENTED_EDGE('',*,*,#3325,.T.);
#4543=ORIENTED_EDGE('',*,*,#3326,.T.);
#4544=ORIENTED_EDGE('',*,*,#3327,.T.);
#4545=ORIENTED_EDGE('',*,*,#3328,.T.);
#4546=ORIENTED_EDGE('',*,*,#3329,.T.);
#4547=ORIENTED_EDGE('',*,*,#3330,.T.);
#4548=ORIENTED_EDGE('',*,*,#3331,.T.);
#4549=ORIENTED_EDGE('',*,*,#3332,.T.);
#4550=ORIENTED_EDGE('',*,*,#3333,.T.);
#4551=ORIENTED_EDGE('',*,*,#3334,.F.);
#4552=ORIENTED_EDGE('',*,*,#3335,.F.);
#4553=ORIENTED_EDGE('',*,*,#3326,.F.);
#4554=ORIENTED_EDGE('',*,*,#3335,.T.);
#4555=ORIENTED_EDGE('',*,*,#3336,.F.);
#4556=ORIENTED_EDGE('',*,*,#3337,.F.);
#4557=ORIENTED_EDGE('',*,*,#3327,.F.);
#4558=ORIENTED_EDGE('',*,*,#3322,.T.);
#4559=ORIENTED_EDGE('',*,*,#3337,.T.);
#4560=ORIENTED_EDGE('',*,*,#3338,.F.);
#4561=ORIENTED_EDGE('',*,*,#3339,.F.);
#4562=ORIENTED_EDGE('',*,*,#3328,.F.);
#4563=ORIENTED_EDGE('',*,*,#3339,.T.);
#4564=ORIENTED_EDGE('',*,*,#3340,.F.);
#4565=ORIENTED_EDGE('',*,*,#3341,.F.);
#4566=ORIENTED_EDGE('',*,*,#3329,.F.);
#4567=ORIENTED_EDGE('',*,*,#3321,.T.);
#4568=ORIENTED_EDGE('',*,*,#3324,.T.);
#4569=ORIENTED_EDGE('',*,*,#3341,.T.);
#4570=ORIENTED_EDGE('',*,*,#3342,.F.);
#4571=ORIENTED_EDGE('',*,*,#3343,.F.);
#4572=ORIENTED_EDGE('',*,*,#3330,.F.);
#4573=ORIENTED_EDGE('',*,*,#3343,.T.);
#4574=ORIENTED_EDGE('',*,*,#3344,.F.);
#4575=ORIENTED_EDGE('',*,*,#3345,.F.);
#4576=ORIENTED_EDGE('',*,*,#3331,.F.);
#4577=ORIENTED_EDGE('',*,*,#3319,.T.);
#4578=ORIENTED_EDGE('',*,*,#3345,.T.);
#4579=ORIENTED_EDGE('',*,*,#3346,.F.);
#4580=ORIENTED_EDGE('',*,*,#3347,.F.);
#4581=ORIENTED_EDGE('',*,*,#3332,.F.);
#4582=ORIENTED_EDGE('',*,*,#3347,.T.);
#4583=ORIENTED_EDGE('',*,*,#3348,.F.);
#4584=ORIENTED_EDGE('',*,*,#3333,.F.);
#4585=ORIENTED_EDGE('',*,*,#3325,.F.);
#4586=ORIENTED_EDGE('',*,*,#3348,.T.);
#4587=ORIENTED_EDGE('',*,*,#3346,.T.);
#4588=ORIENTED_EDGE('',*,*,#3344,.T.);
#4589=ORIENTED_EDGE('',*,*,#3342,.T.);
#4590=ORIENTED_EDGE('',*,*,#3340,.T.);
#4591=ORIENTED_EDGE('',*,*,#3338,.T.);
#4592=ORIENTED_EDGE('',*,*,#3336,.T.);
#4593=ORIENTED_EDGE('',*,*,#3334,.T.);
#4594=ORIENTED_EDGE('',*,*,#3349,.F.);
#4595=ORIENTED_EDGE('',*,*,#3350,.T.);
#4596=ORIENTED_EDGE('',*,*,#3351,.T.);
#4597=ORIENTED_EDGE('',*,*,#3350,.F.);
#4598=ORIENTED_EDGE('',*,*,#3351,.F.);
#4599=ORIENTED_EDGE('',*,*,#3352,.F.);
#4600=ORIENTED_EDGE('',*,*,#3353,.T.);
#4601=ORIENTED_EDGE('',*,*,#3354,.T.);
#4602=ORIENTED_EDGE('',*,*,#3353,.F.);
#4603=ORIENTED_EDGE('',*,*,#3354,.F.);
#4604=ORIENTED_EDGE('',*,*,#3355,.F.);
#4605=ORIENTED_EDGE('',*,*,#3356,.T.);
#4606=ORIENTED_EDGE('',*,*,#3357,.T.);
#4607=ORIENTED_EDGE('',*,*,#3356,.F.);
#4608=ORIENTED_EDGE('',*,*,#3357,.F.);
#4609=ORIENTED_EDGE('',*,*,#3358,.T.);
#4610=ORIENTED_EDGE('',*,*,#3359,.T.);
#4611=ORIENTED_EDGE('',*,*,#3360,.T.);
#4612=ORIENTED_EDGE('',*,*,#3361,.T.);
#4613=ORIENTED_EDGE('',*,*,#3362,.T.);
#4614=ORIENTED_EDGE('',*,*,#3359,.F.);
#4615=ORIENTED_EDGE('',*,*,#3363,.T.);
#4616=ORIENTED_EDGE('',*,*,#3364,.T.);
#4617=ORIENTED_EDGE('',*,*,#3365,.T.);
#4618=ORIENTED_EDGE('',*,*,#3361,.F.);
#4619=ORIENTED_EDGE('',*,*,#3366,.T.);
#4620=ORIENTED_EDGE('',*,*,#3367,.T.);
#4621=ORIENTED_EDGE('',*,*,#3368,.T.);
#4622=ORIENTED_EDGE('',*,*,#3364,.F.);
#4623=ORIENTED_EDGE('',*,*,#3369,.T.);
#4624=ORIENTED_EDGE('',*,*,#3367,.F.);
#4625=ORIENTED_EDGE('',*,*,#3366,.F.);
#4626=ORIENTED_EDGE('',*,*,#3370,.T.);
#4627=ORIENTED_EDGE('',*,*,#3371,.F.);
#4628=ORIENTED_EDGE('',*,*,#3372,.F.);
#4629=ORIENTED_EDGE('',*,*,#3373,.F.);
#4630=ORIENTED_EDGE('',*,*,#3374,.F.);
#4631=ORIENTED_EDGE('',*,*,#3360,.F.);
#4632=ORIENTED_EDGE('',*,*,#3375,.F.);
#4633=ORIENTED_EDGE('',*,*,#3376,.F.);
#4634=ORIENTED_EDGE('',*,*,#3377,.F.);
#4635=ORIENTED_EDGE('',*,*,#3378,.F.);
#4636=ORIENTED_EDGE('',*,*,#3379,.F.);
#4637=ORIENTED_EDGE('',*,*,#3380,.F.);
#4638=ORIENTED_EDGE('',*,*,#3381,.F.);
#4639=ORIENTED_EDGE('',*,*,#3382,.F.);
#4640=ORIENTED_EDGE('',*,*,#3383,.F.);
#4641=ORIENTED_EDGE('',*,*,#3384,.F.);
#4642=ORIENTED_EDGE('',*,*,#3370,.F.);
#4643=ORIENTED_EDGE('',*,*,#3358,.F.);
#4644=ORIENTED_EDGE('',*,*,#3365,.F.);
#4645=ORIENTED_EDGE('',*,*,#3369,.F.);
#4646=ORIENTED_EDGE('',*,*,#3363,.F.);
#4647=ORIENTED_EDGE('',*,*,#3349,.T.);
#4648=ORIENTED_EDGE('',*,*,#3352,.T.);
#4649=ORIENTED_EDGE('',*,*,#3355,.T.);
#4650=ORIENTED_EDGE('',*,*,#3362,.F.);
#4651=ORIENTED_EDGE('',*,*,#3385,.F.);
#4652=ORIENTED_EDGE('',*,*,#3386,.F.);
#4653=ORIENTED_EDGE('',*,*,#3387,.F.);
#4654=ORIENTED_EDGE('',*,*,#3388,.F.);
#4655=ORIENTED_EDGE('',*,*,#3375,.T.);
#4656=ORIENTED_EDGE('',*,*,#3368,.F.);
#4657=ORIENTED_EDGE('',*,*,#3374,.T.);
#4658=ORIENTED_EDGE('',*,*,#3389,.F.);
#4659=ORIENTED_EDGE('',*,*,#3390,.F.);
#4660=ORIENTED_EDGE('',*,*,#3391,.F.);
#4661=ORIENTED_EDGE('',*,*,#3392,.F.);
#4662=ORIENTED_EDGE('',*,*,#3393,.F.);
#4663=ORIENTED_EDGE('',*,*,#3394,.F.);
#4664=ORIENTED_EDGE('',*,*,#3395,.F.);
#4665=ORIENTED_EDGE('',*,*,#3396,.F.);
#4666=ORIENTED_EDGE('',*,*,#3397,.F.);
#4667=ORIENTED_EDGE('',*,*,#3385,.T.);
#4668=ORIENTED_EDGE('',*,*,#3373,.T.);
#4669=ORIENTED_EDGE('',*,*,#3398,.T.);
#4670=ORIENTED_EDGE('',*,*,#3399,.T.);
#4671=ORIENTED_EDGE('',*,*,#3389,.T.);
#4672=ORIENTED_EDGE('',*,*,#3386,.T.);
#4673=ORIENTED_EDGE('',*,*,#3397,.T.);
#4674=ORIENTED_EDGE('',*,*,#3400,.F.);
#4675=ORIENTED_EDGE('',*,*,#3401,.T.);
#4676=ORIENTED_EDGE('',*,*,#3372,.T.);
#4677=ORIENTED_EDGE('',*,*,#3402,.F.);
#4678=ORIENTED_EDGE('',*,*,#3403,.F.);
#4679=ORIENTED_EDGE('',*,*,#3398,.F.);
#4680=ORIENTED_EDGE('',*,*,#3371,.T.);
#4681=ORIENTED_EDGE('',*,*,#3384,.T.);
#4682=ORIENTED_EDGE('',*,*,#3404,.T.);
#4683=ORIENTED_EDGE('',*,*,#3402,.T.);
#4684=ORIENTED_EDGE('',*,*,#3405,.T.);
#4685=ORIENTED_EDGE('',*,*,#3406,.T.);
#4686=ORIENTED_EDGE('',*,*,#3391,.T.);
#4687=ORIENTED_EDGE('',*,*,#3407,.T.);
#4688=ORIENTED_EDGE('',*,*,#3408,.T.);
#4689=ORIENTED_EDGE('',*,*,#3409,.T.);
#4690=ORIENTED_EDGE('',*,*,#3392,.T.);
#4691=ORIENTED_EDGE('',*,*,#3406,.F.);
#4692=ORIENTED_EDGE('',*,*,#3410,.T.);
#4693=ORIENTED_EDGE('',*,*,#3411,.T.);
#4694=ORIENTED_EDGE('',*,*,#3393,.T.);
#4695=ORIENTED_EDGE('',*,*,#3409,.F.);
#4696=ORIENTED_EDGE('',*,*,#3412,.T.);
#4697=ORIENTED_EDGE('',*,*,#3413,.T.);
#4698=ORIENTED_EDGE('',*,*,#3394,.T.);
#4699=ORIENTED_EDGE('',*,*,#3411,.F.);
#4700=ORIENTED_EDGE('',*,*,#3395,.T.);
#4701=ORIENTED_EDGE('',*,*,#3413,.F.);
#4702=ORIENTED_EDGE('',*,*,#3414,.T.);
#4703=ORIENTED_EDGE('',*,*,#3415,.T.);
#4704=ORIENTED_EDGE('',*,*,#3396,.T.);
#4705=ORIENTED_EDGE('',*,*,#3415,.F.);
#4706=ORIENTED_EDGE('',*,*,#3416,.T.);
#4707=ORIENTED_EDGE('',*,*,#3400,.T.);
#4708=ORIENTED_EDGE('',*,*,#3417,.T.);
#4709=ORIENTED_EDGE('',*,*,#3407,.F.);
#4710=ORIENTED_EDGE('',*,*,#3390,.T.);
#4711=ORIENTED_EDGE('',*,*,#3399,.F.);
#4712=ORIENTED_EDGE('',*,*,#3412,.F.);
#4713=ORIENTED_EDGE('',*,*,#3418,.T.);
#4714=ORIENTED_EDGE('',*,*,#3419,.F.);
#4715=ORIENTED_EDGE('',*,*,#3420,.T.);
#4716=ORIENTED_EDGE('',*,*,#3410,.F.);
#4717=ORIENTED_EDGE('',*,*,#3421,.F.);
#4718=ORIENTED_EDGE('',*,*,#3422,.F.);
#4719=ORIENTED_EDGE('',*,*,#3418,.F.);
#4720=ORIENTED_EDGE('',*,*,#3408,.F.);
#4721=ORIENTED_EDGE('',*,*,#3423,.T.);
#4722=ORIENTED_EDGE('',*,*,#3424,.F.);
#4723=ORIENTED_EDGE('',*,*,#3421,.T.);
#4724=ORIENTED_EDGE('',*,*,#3405,.F.);
#4725=ORIENTED_EDGE('',*,*,#3425,.F.);
#4726=ORIENTED_EDGE('',*,*,#3426,.F.);
#4727=ORIENTED_EDGE('',*,*,#3423,.F.);
#4728=ORIENTED_EDGE('',*,*,#3382,.T.);
#4729=ORIENTED_EDGE('',*,*,#3427,.T.);
#4730=ORIENTED_EDGE('',*,*,#3426,.T.);
#4731=ORIENTED_EDGE('',*,*,#3428,.F.);
#4732=ORIENTED_EDGE('',*,*,#3381,.T.);
#4733=ORIENTED_EDGE('',*,*,#3429,.T.);
#4734=ORIENTED_EDGE('',*,*,#3424,.T.);
#4735=ORIENTED_EDGE('',*,*,#3427,.F.);
#4736=ORIENTED_EDGE('',*,*,#3380,.T.);
#4737=ORIENTED_EDGE('',*,*,#3430,.T.);
#4738=ORIENTED_EDGE('',*,*,#3422,.T.);
#4739=ORIENTED_EDGE('',*,*,#3429,.F.);
#4740=ORIENTED_EDGE('',*,*,#3419,.T.);
#4741=ORIENTED_EDGE('',*,*,#3430,.F.);
#4742=ORIENTED_EDGE('',*,*,#3379,.T.);
#4743=ORIENTED_EDGE('',*,*,#3431,.T.);
#4744=ORIENTED_EDGE('',*,*,#3432,.T.);
#4745=ORIENTED_EDGE('',*,*,#3431,.F.);
#4746=ORIENTED_EDGE('',*,*,#3378,.T.);
#4747=ORIENTED_EDGE('',*,*,#3433,.T.);
#4748=ORIENTED_EDGE('',*,*,#3434,.T.);
#4749=ORIENTED_EDGE('',*,*,#3433,.F.);
#4750=ORIENTED_EDGE('',*,*,#3377,.T.);
#4751=ORIENTED_EDGE('',*,*,#3435,.T.);
#4752=ORIENTED_EDGE('',*,*,#3388,.T.);
#4753=ORIENTED_EDGE('',*,*,#3436,.T.);
#4754=ORIENTED_EDGE('',*,*,#3435,.F.);
#4755=ORIENTED_EDGE('',*,*,#3376,.T.);
#4756=ORIENTED_EDGE('',*,*,#3437,.T.);
#4757=ORIENTED_EDGE('',*,*,#3404,.F.);
#4758=ORIENTED_EDGE('',*,*,#3383,.T.);
#4759=ORIENTED_EDGE('',*,*,#3428,.T.);
#4760=ORIENTED_EDGE('',*,*,#3416,.F.);
#4761=ORIENTED_EDGE('',*,*,#3438,.T.);
#4762=ORIENTED_EDGE('',*,*,#3434,.F.);
#4763=ORIENTED_EDGE('',*,*,#3439,.T.);
#4764=ORIENTED_EDGE('',*,*,#3387,.T.);
#4765=ORIENTED_EDGE('',*,*,#3401,.F.);
#4766=ORIENTED_EDGE('',*,*,#3439,.F.);
#4767=ORIENTED_EDGE('',*,*,#3436,.F.);
#4768=ORIENTED_EDGE('',*,*,#3417,.F.);
#4769=ORIENTED_EDGE('',*,*,#3403,.T.);
#4770=ORIENTED_EDGE('',*,*,#3437,.F.);
#4771=ORIENTED_EDGE('',*,*,#3425,.T.);
#4772=ORIENTED_EDGE('',*,*,#3414,.F.);
#4773=ORIENTED_EDGE('',*,*,#3420,.F.);
#4774=ORIENTED_EDGE('',*,*,#3432,.F.);
#4775=ORIENTED_EDGE('',*,*,#3438,.F.);
#4776=ORIENTED_EDGE('',*,*,#3440,.F.);
#4777=ORIENTED_EDGE('',*,*,#3441,.T.);
#4778=ORIENTED_EDGE('',*,*,#3442,.F.);
#4779=ORIENTED_EDGE('',*,*,#3441,.F.);
#4780=ORIENTED_EDGE('',*,*,#3443,.F.);
#4781=ORIENTED_EDGE('',*,*,#3444,.T.);
#4782=ORIENTED_EDGE('',*,*,#3445,.F.);
#4783=ORIENTED_EDGE('',*,*,#3444,.F.);
#4784=ORIENTED_EDGE('',*,*,#3446,.F.);
#4785=ORIENTED_EDGE('',*,*,#3447,.T.);
#4786=ORIENTED_EDGE('',*,*,#3448,.F.);
#4787=ORIENTED_EDGE('',*,*,#3447,.F.);
#4788=ORIENTED_EDGE('',*,*,#3449,.F.);
#4789=ORIENTED_EDGE('',*,*,#3450,.T.);
#4790=ORIENTED_EDGE('',*,*,#3451,.F.);
#4791=ORIENTED_EDGE('',*,*,#3450,.F.);
#4792=ORIENTED_EDGE('',*,*,#3452,.T.);
#4793=ORIENTED_EDGE('',*,*,#3453,.T.);
#4794=ORIENTED_EDGE('',*,*,#3454,.T.);
#4795=ORIENTED_EDGE('',*,*,#3455,.F.);
#4796=ORIENTED_EDGE('',*,*,#3456,.T.);
#4797=ORIENTED_EDGE('',*,*,#3457,.T.);
#4798=ORIENTED_EDGE('',*,*,#3458,.T.);
#4799=ORIENTED_EDGE('',*,*,#3459,.T.);
#4800=ORIENTED_EDGE('',*,*,#3460,.T.);
#4801=ORIENTED_EDGE('',*,*,#3461,.T.);
#4802=ORIENTED_EDGE('',*,*,#3462,.T.);
#4803=ORIENTED_EDGE('',*,*,#3457,.F.);
#4804=ORIENTED_EDGE('',*,*,#3463,.T.);
#4805=ORIENTED_EDGE('',*,*,#3464,.T.);
#4806=ORIENTED_EDGE('',*,*,#3465,.T.);
#4807=ORIENTED_EDGE('',*,*,#3466,.T.);
#4808=ORIENTED_EDGE('',*,*,#3467,.T.);
#4809=ORIENTED_EDGE('',*,*,#3468,.T.);
#4810=ORIENTED_EDGE('',*,*,#3469,.T.);
#4811=ORIENTED_EDGE('',*,*,#3461,.F.);
#4812=ORIENTED_EDGE('',*,*,#3470,.T.);
#4813=ORIENTED_EDGE('',*,*,#3468,.F.);
#4814=ORIENTED_EDGE('',*,*,#3471,.T.);
#4815=ORIENTED_EDGE('',*,*,#3464,.F.);
#4816=ORIENTED_EDGE('',*,*,#3472,.T.);
#4817=ORIENTED_EDGE('',*,*,#3466,.F.);
#4818=ORIENTED_EDGE('',*,*,#3473,.T.);
#4819=ORIENTED_EDGE('',*,*,#3474,.T.);
#4820=ORIENTED_EDGE('',*,*,#3475,.T.);
#4821=ORIENTED_EDGE('',*,*,#3474,.F.);
#4822=ORIENTED_EDGE('',*,*,#3476,.T.);
#4823=ORIENTED_EDGE('',*,*,#3477,.T.);
#4824=ORIENTED_EDGE('',*,*,#3478,.T.);
#4825=ORIENTED_EDGE('',*,*,#3459,.F.);
#4826=ORIENTED_EDGE('',*,*,#3479,.T.);
#4827=ORIENTED_EDGE('',*,*,#3453,.F.);
#4828=ORIENTED_EDGE('',*,*,#3480,.T.);
#4829=ORIENTED_EDGE('',*,*,#3477,.F.);
#4830=ORIENTED_EDGE('',*,*,#3481,.T.);
#4831=ORIENTED_EDGE('',*,*,#3482,.T.);
#4832=ORIENTED_EDGE('',*,*,#3483,.T.);
#4833=ORIENTED_EDGE('',*,*,#3482,.F.);
#4834=ORIENTED_EDGE('',*,*,#3484,.T.);
#4835=ORIENTED_EDGE('',*,*,#3485,.T.);
#4836=ORIENTED_EDGE('',*,*,#3486,.T.);
#4837=ORIENTED_EDGE('',*,*,#3485,.F.);
#4838=ORIENTED_EDGE('',*,*,#3487,.T.);
#4839=ORIENTED_EDGE('',*,*,#3455,.T.);
#4840=ORIENTED_EDGE('',*,*,#3479,.F.);
#4841=ORIENTED_EDGE('',*,*,#3488,.T.);
#4842=ORIENTED_EDGE('',*,*,#3489,.F.);
#4843=ORIENTED_EDGE('',*,*,#3490,.T.);
#4844=ORIENTED_EDGE('',*,*,#3458,.F.);
#4845=ORIENTED_EDGE('',*,*,#3491,.T.);
#4846=ORIENTED_EDGE('',*,*,#3492,.F.);
#4847=ORIENTED_EDGE('',*,*,#3488,.F.);
#4848=ORIENTED_EDGE('',*,*,#3462,.F.);
#4849=ORIENTED_EDGE('',*,*,#3493,.T.);
#4850=ORIENTED_EDGE('',*,*,#3494,.F.);
#4851=ORIENTED_EDGE('',*,*,#3491,.F.);
#4852=ORIENTED_EDGE('',*,*,#3469,.F.);
#4853=ORIENTED_EDGE('',*,*,#3495,.F.);
#4854=ORIENTED_EDGE('',*,*,#3496,.F.);
#4855=ORIENTED_EDGE('',*,*,#3493,.F.);
#4856=ORIENTED_EDGE('',*,*,#3470,.F.);
#4857=ORIENTED_EDGE('',*,*,#3497,.T.);
#4858=ORIENTED_EDGE('',*,*,#3498,.F.);
#4859=ORIENTED_EDGE('',*,*,#3495,.T.);
#4860=ORIENTED_EDGE('',*,*,#3463,.F.);
#4861=ORIENTED_EDGE('',*,*,#3499,.T.);
#4862=ORIENTED_EDGE('',*,*,#3500,.F.);
#4863=ORIENTED_EDGE('',*,*,#3497,.F.);
#4864=ORIENTED_EDGE('',*,*,#3465,.F.);
#4865=ORIENTED_EDGE('',*,*,#3471,.F.);
#4866=ORIENTED_EDGE('',*,*,#3467,.F.);
#4867=ORIENTED_EDGE('',*,*,#3460,.F.);
#4868=ORIENTED_EDGE('',*,*,#3456,.F.);
#4869=ORIENTED_EDGE('',*,*,#3478,.F.);
#4870=ORIENTED_EDGE('',*,*,#3452,.F.);
#4871=ORIENTED_EDGE('',*,*,#3487,.F.);
#4872=ORIENTED_EDGE('',*,*,#3484,.F.);
#4873=ORIENTED_EDGE('',*,*,#3481,.F.);
#4874=ORIENTED_EDGE('',*,*,#3476,.F.);
#4875=ORIENTED_EDGE('',*,*,#3473,.F.);
#4876=ORIENTED_EDGE('',*,*,#3442,.T.);
#4877=ORIENTED_EDGE('',*,*,#3445,.T.);
#4878=ORIENTED_EDGE('',*,*,#3448,.T.);
#4879=ORIENTED_EDGE('',*,*,#3451,.T.);
#4880=ORIENTED_EDGE('',*,*,#3501,.T.);
#4881=ORIENTED_EDGE('',*,*,#3502,.T.);
#4882=ORIENTED_EDGE('',*,*,#3503,.T.);
#4883=ORIENTED_EDGE('',*,*,#3504,.F.);
#4884=ORIENTED_EDGE('',*,*,#3505,.T.);
#4885=ORIENTED_EDGE('',*,*,#3506,.T.);
#4886=ORIENTED_EDGE('',*,*,#3507,.T.);
#4887=ORIENTED_EDGE('',*,*,#3502,.F.);
#4888=ORIENTED_EDGE('',*,*,#3508,.T.);
#4889=ORIENTED_EDGE('',*,*,#3509,.T.);
#4890=ORIENTED_EDGE('',*,*,#3510,.T.);
#4891=ORIENTED_EDGE('',*,*,#3506,.F.);
#4892=ORIENTED_EDGE('',*,*,#3511,.T.);
#4893=ORIENTED_EDGE('',*,*,#3512,.T.);
#4894=ORIENTED_EDGE('',*,*,#3513,.T.);
#4895=ORIENTED_EDGE('',*,*,#3509,.F.);
#4896=ORIENTED_EDGE('',*,*,#3514,.T.);
#4897=ORIENTED_EDGE('',*,*,#3515,.T.);
#4898=ORIENTED_EDGE('',*,*,#3516,.T.);
#4899=ORIENTED_EDGE('',*,*,#3512,.F.);
#4900=ORIENTED_EDGE('',*,*,#3517,.T.);
#4901=ORIENTED_EDGE('',*,*,#3518,.T.);
#4902=ORIENTED_EDGE('',*,*,#3500,.T.);
#4903=ORIENTED_EDGE('',*,*,#3515,.F.);
#4904=ORIENTED_EDGE('',*,*,#3498,.T.);
#4905=ORIENTED_EDGE('',*,*,#3518,.F.);
#4906=ORIENTED_EDGE('',*,*,#3519,.T.);
#4907=ORIENTED_EDGE('',*,*,#3520,.T.);
#4908=ORIENTED_EDGE('',*,*,#3496,.T.);
#4909=ORIENTED_EDGE('',*,*,#3520,.F.);
#4910=ORIENTED_EDGE('',*,*,#3521,.T.);
#4911=ORIENTED_EDGE('',*,*,#3522,.T.);
#4912=ORIENTED_EDGE('',*,*,#3494,.T.);
#4913=ORIENTED_EDGE('',*,*,#3522,.F.);
#4914=ORIENTED_EDGE('',*,*,#3523,.T.);
#4915=ORIENTED_EDGE('',*,*,#3524,.T.);
#4916=ORIENTED_EDGE('',*,*,#3492,.T.);
#4917=ORIENTED_EDGE('',*,*,#3524,.F.);
#4918=ORIENTED_EDGE('',*,*,#3525,.T.);
#4919=ORIENTED_EDGE('',*,*,#3526,.T.);
#4920=ORIENTED_EDGE('',*,*,#3489,.T.);
#4921=ORIENTED_EDGE('',*,*,#3526,.F.);
#4922=ORIENTED_EDGE('',*,*,#3527,.T.);
#4923=ORIENTED_EDGE('',*,*,#3528,.T.);
#4924=ORIENTED_EDGE('',*,*,#3529,.T.);
#4925=ORIENTED_EDGE('',*,*,#3528,.F.);
#4926=ORIENTED_EDGE('',*,*,#3530,.T.);
#4927=ORIENTED_EDGE('',*,*,#3504,.T.);
#4928=ORIENTED_EDGE('',*,*,#3454,.F.);
#4929=ORIENTED_EDGE('',*,*,#3490,.F.);
#4930=ORIENTED_EDGE('',*,*,#3529,.F.);
#4931=ORIENTED_EDGE('',*,*,#3531,.F.);
#4932=ORIENTED_EDGE('',*,*,#3486,.F.);
#4933=ORIENTED_EDGE('',*,*,#3531,.T.);
#4934=ORIENTED_EDGE('',*,*,#3503,.F.);
#4935=ORIENTED_EDGE('',*,*,#3532,.F.);
#4936=ORIENTED_EDGE('',*,*,#3501,.F.);
#4937=ORIENTED_EDGE('',*,*,#3530,.F.);
#4938=ORIENTED_EDGE('',*,*,#3527,.F.);
#4939=ORIENTED_EDGE('',*,*,#3525,.F.);
#4940=ORIENTED_EDGE('',*,*,#3523,.F.);
#4941=ORIENTED_EDGE('',*,*,#3521,.F.);
#4942=ORIENTED_EDGE('',*,*,#3519,.F.);
#4943=ORIENTED_EDGE('',*,*,#3517,.F.);
#4944=ORIENTED_EDGE('',*,*,#3514,.F.);
#4945=ORIENTED_EDGE('',*,*,#3511,.F.);
#4946=ORIENTED_EDGE('',*,*,#3508,.F.);
#4947=ORIENTED_EDGE('',*,*,#3505,.F.);
#4948=ORIENTED_EDGE('',*,*,#3440,.T.);
#4949=ORIENTED_EDGE('',*,*,#3443,.T.);
#4950=ORIENTED_EDGE('',*,*,#3446,.T.);
#4951=ORIENTED_EDGE('',*,*,#3449,.T.);
#4952=ORIENTED_EDGE('',*,*,#3483,.F.);
#4953=ORIENTED_EDGE('',*,*,#3532,.T.);
#4954=ORIENTED_EDGE('',*,*,#3507,.F.);
#4955=ORIENTED_EDGE('',*,*,#3533,.F.);
#4956=ORIENTED_EDGE('',*,*,#3480,.F.);
#4957=ORIENTED_EDGE('',*,*,#3533,.T.);
#4958=ORIENTED_EDGE('',*,*,#3510,.F.);
#4959=ORIENTED_EDGE('',*,*,#3534,.F.);
#4960=ORIENTED_EDGE('',*,*,#3475,.F.);
#4961=ORIENTED_EDGE('',*,*,#3534,.T.);
#4962=ORIENTED_EDGE('',*,*,#3513,.F.);
#4963=ORIENTED_EDGE('',*,*,#3535,.F.);
#4964=ORIENTED_EDGE('',*,*,#3472,.F.);
#4965=ORIENTED_EDGE('',*,*,#3535,.T.);
#4966=ORIENTED_EDGE('',*,*,#3516,.F.);
#4967=ORIENTED_EDGE('',*,*,#3499,.F.);
#4968=ORIENTED_EDGE('',*,*,#3536,.F.);
#4969=ORIENTED_EDGE('',*,*,#3537,.T.);
#4970=ORIENTED_EDGE('',*,*,#3538,.F.);
#4971=ORIENTED_EDGE('',*,*,#3537,.F.);
#4972=ORIENTED_EDGE('',*,*,#3539,.F.);
#4973=ORIENTED_EDGE('',*,*,#3540,.T.);
#4974=ORIENTED_EDGE('',*,*,#3541,.F.);
#4975=ORIENTED_EDGE('',*,*,#3540,.F.);
#4976=ORIENTED_EDGE('',*,*,#3542,.F.);
#4977=ORIENTED_EDGE('',*,*,#3543,.T.);
#4978=ORIENTED_EDGE('',*,*,#3544,.F.);
#4979=ORIENTED_EDGE('',*,*,#3543,.F.);
#4980=ORIENTED_EDGE('',*,*,#3545,.F.);
#4981=ORIENTED_EDGE('',*,*,#3546,.T.);
#4982=ORIENTED_EDGE('',*,*,#3547,.F.);
#4983=ORIENTED_EDGE('',*,*,#3546,.F.);
#4984=ORIENTED_EDGE('',*,*,#3548,.T.);
#4985=ORIENTED_EDGE('',*,*,#3549,.T.);
#4986=ORIENTED_EDGE('',*,*,#3550,.T.);
#4987=ORIENTED_EDGE('',*,*,#3551,.F.);
#4988=ORIENTED_EDGE('',*,*,#3552,.T.);
#4989=ORIENTED_EDGE('',*,*,#3553,.T.);
#4990=ORIENTED_EDGE('',*,*,#3554,.T.);
#4991=ORIENTED_EDGE('',*,*,#3555,.T.);
#4992=ORIENTED_EDGE('',*,*,#3556,.T.);
#4993=ORIENTED_EDGE('',*,*,#3557,.T.);
#4994=ORIENTED_EDGE('',*,*,#3558,.T.);
#4995=ORIENTED_EDGE('',*,*,#3553,.F.);
#4996=ORIENTED_EDGE('',*,*,#3559,.T.);
#4997=ORIENTED_EDGE('',*,*,#3560,.T.);
#4998=ORIENTED_EDGE('',*,*,#3561,.T.);
#4999=ORIENTED_EDGE('',*,*,#3562,.T.);
#5000=ORIENTED_EDGE('',*,*,#3563,.T.);
#5001=ORIENTED_EDGE('',*,*,#3564,.T.);
#5002=ORIENTED_EDGE('',*,*,#3565,.T.);
#5003=ORIENTED_EDGE('',*,*,#3557,.F.);
#5004=ORIENTED_EDGE('',*,*,#3566,.T.);
#5005=ORIENTED_EDGE('',*,*,#3564,.F.);
#5006=ORIENTED_EDGE('',*,*,#3567,.T.);
#5007=ORIENTED_EDGE('',*,*,#3560,.F.);
#5008=ORIENTED_EDGE('',*,*,#3568,.T.);
#5009=ORIENTED_EDGE('',*,*,#3562,.F.);
#5010=ORIENTED_EDGE('',*,*,#3569,.T.);
#5011=ORIENTED_EDGE('',*,*,#3570,.T.);
#5012=ORIENTED_EDGE('',*,*,#3571,.T.);
#5013=ORIENTED_EDGE('',*,*,#3570,.F.);
#5014=ORIENTED_EDGE('',*,*,#3572,.T.);
#5015=ORIENTED_EDGE('',*,*,#3573,.T.);
#5016=ORIENTED_EDGE('',*,*,#3574,.T.);
#5017=ORIENTED_EDGE('',*,*,#3555,.F.);
#5018=ORIENTED_EDGE('',*,*,#3575,.T.);
#5019=ORIENTED_EDGE('',*,*,#3549,.F.);
#5020=ORIENTED_EDGE('',*,*,#3576,.T.);
#5021=ORIENTED_EDGE('',*,*,#3573,.F.);
#5022=ORIENTED_EDGE('',*,*,#3577,.T.);
#5023=ORIENTED_EDGE('',*,*,#3578,.T.);
#5024=ORIENTED_EDGE('',*,*,#3579,.T.);
#5025=ORIENTED_EDGE('',*,*,#3578,.F.);
#5026=ORIENTED_EDGE('',*,*,#3580,.T.);
#5027=ORIENTED_EDGE('',*,*,#3581,.T.);
#5028=ORIENTED_EDGE('',*,*,#3582,.T.);
#5029=ORIENTED_EDGE('',*,*,#3581,.F.);
#5030=ORIENTED_EDGE('',*,*,#3583,.T.);
#5031=ORIENTED_EDGE('',*,*,#3551,.T.);
#5032=ORIENTED_EDGE('',*,*,#3575,.F.);
#5033=ORIENTED_EDGE('',*,*,#3584,.T.);
#5034=ORIENTED_EDGE('',*,*,#3585,.F.);
#5035=ORIENTED_EDGE('',*,*,#3586,.T.);
#5036=ORIENTED_EDGE('',*,*,#3554,.F.);
#5037=ORIENTED_EDGE('',*,*,#3587,.T.);
#5038=ORIENTED_EDGE('',*,*,#3588,.F.);
#5039=ORIENTED_EDGE('',*,*,#3584,.F.);
#5040=ORIENTED_EDGE('',*,*,#3558,.F.);
#5041=ORIENTED_EDGE('',*,*,#3589,.T.);
#5042=ORIENTED_EDGE('',*,*,#3590,.F.);
#5043=ORIENTED_EDGE('',*,*,#3587,.F.);
#5044=ORIENTED_EDGE('',*,*,#3565,.F.);
#5045=ORIENTED_EDGE('',*,*,#3591,.F.);
#5046=ORIENTED_EDGE('',*,*,#3592,.F.);
#5047=ORIENTED_EDGE('',*,*,#3589,.F.);
#5048=ORIENTED_EDGE('',*,*,#3566,.F.);
#5049=ORIENTED_EDGE('',*,*,#3593,.T.);
#5050=ORIENTED_EDGE('',*,*,#3594,.F.);
#5051=ORIENTED_EDGE('',*,*,#3591,.T.);
#5052=ORIENTED_EDGE('',*,*,#3559,.F.);
#5053=ORIENTED_EDGE('',*,*,#3595,.T.);
#5054=ORIENTED_EDGE('',*,*,#3596,.F.);
#5055=ORIENTED_EDGE('',*,*,#3593,.F.);
#5056=ORIENTED_EDGE('',*,*,#3561,.F.);
#5057=ORIENTED_EDGE('',*,*,#3567,.F.);
#5058=ORIENTED_EDGE('',*,*,#3563,.F.);
#5059=ORIENTED_EDGE('',*,*,#3556,.F.);
#5060=ORIENTED_EDGE('',*,*,#3552,.F.);
#5061=ORIENTED_EDGE('',*,*,#3574,.F.);
#5062=ORIENTED_EDGE('',*,*,#3548,.F.);
#5063=ORIENTED_EDGE('',*,*,#3583,.F.);
#5064=ORIENTED_EDGE('',*,*,#3580,.F.);
#5065=ORIENTED_EDGE('',*,*,#3577,.F.);
#5066=ORIENTED_EDGE('',*,*,#3572,.F.);
#5067=ORIENTED_EDGE('',*,*,#3569,.F.);
#5068=ORIENTED_EDGE('',*,*,#3538,.T.);
#5069=ORIENTED_EDGE('',*,*,#3541,.T.);
#5070=ORIENTED_EDGE('',*,*,#3544,.T.);
#5071=ORIENTED_EDGE('',*,*,#3547,.T.);
#5072=ORIENTED_EDGE('',*,*,#3597,.T.);
#5073=ORIENTED_EDGE('',*,*,#3598,.T.);
#5074=ORIENTED_EDGE('',*,*,#3599,.T.);
#5075=ORIENTED_EDGE('',*,*,#3600,.F.);
#5076=ORIENTED_EDGE('',*,*,#3601,.T.);
#5077=ORIENTED_EDGE('',*,*,#3602,.T.);
#5078=ORIENTED_EDGE('',*,*,#3603,.T.);
#5079=ORIENTED_EDGE('',*,*,#3598,.F.);
#5080=ORIENTED_EDGE('',*,*,#3604,.T.);
#5081=ORIENTED_EDGE('',*,*,#3605,.T.);
#5082=ORIENTED_EDGE('',*,*,#3606,.T.);
#5083=ORIENTED_EDGE('',*,*,#3602,.F.);
#5084=ORIENTED_EDGE('',*,*,#3607,.T.);
#5085=ORIENTED_EDGE('',*,*,#3608,.T.);
#5086=ORIENTED_EDGE('',*,*,#3609,.T.);
#5087=ORIENTED_EDGE('',*,*,#3605,.F.);
#5088=ORIENTED_EDGE('',*,*,#3610,.T.);
#5089=ORIENTED_EDGE('',*,*,#3611,.T.);
#5090=ORIENTED_EDGE('',*,*,#3612,.T.);
#5091=ORIENTED_EDGE('',*,*,#3608,.F.);
#5092=ORIENTED_EDGE('',*,*,#3613,.T.);
#5093=ORIENTED_EDGE('',*,*,#3614,.T.);
#5094=ORIENTED_EDGE('',*,*,#3596,.T.);
#5095=ORIENTED_EDGE('',*,*,#3611,.F.);
#5096=ORIENTED_EDGE('',*,*,#3594,.T.);
#5097=ORIENTED_EDGE('',*,*,#3614,.F.);
#5098=ORIENTED_EDGE('',*,*,#3615,.T.);
#5099=ORIENTED_EDGE('',*,*,#3616,.T.);
#5100=ORIENTED_EDGE('',*,*,#3592,.T.);
#5101=ORIENTED_EDGE('',*,*,#3616,.F.);
#5102=ORIENTED_EDGE('',*,*,#3617,.T.);
#5103=ORIENTED_EDGE('',*,*,#3618,.T.);
#5104=ORIENTED_EDGE('',*,*,#3590,.T.);
#5105=ORIENTED_EDGE('',*,*,#3618,.F.);
#5106=ORIENTED_EDGE('',*,*,#3619,.T.);
#5107=ORIENTED_EDGE('',*,*,#3620,.T.);
#5108=ORIENTED_EDGE('',*,*,#3588,.T.);
#5109=ORIENTED_EDGE('',*,*,#3620,.F.);
#5110=ORIENTED_EDGE('',*,*,#3621,.T.);
#5111=ORIENTED_EDGE('',*,*,#3622,.T.);
#5112=ORIENTED_EDGE('',*,*,#3585,.T.);
#5113=ORIENTED_EDGE('',*,*,#3622,.F.);
#5114=ORIENTED_EDGE('',*,*,#3623,.T.);
#5115=ORIENTED_EDGE('',*,*,#3624,.T.);
#5116=ORIENTED_EDGE('',*,*,#3625,.T.);
#5117=ORIENTED_EDGE('',*,*,#3624,.F.);
#5118=ORIENTED_EDGE('',*,*,#3626,.T.);
#5119=ORIENTED_EDGE('',*,*,#3600,.T.);
#5120=ORIENTED_EDGE('',*,*,#3550,.F.);
#5121=ORIENTED_EDGE('',*,*,#3586,.F.);
#5122=ORIENTED_EDGE('',*,*,#3625,.F.);
#5123=ORIENTED_EDGE('',*,*,#3627,.F.);
#5124=ORIENTED_EDGE('',*,*,#3582,.F.);
#5125=ORIENTED_EDGE('',*,*,#3627,.T.);
#5126=ORIENTED_EDGE('',*,*,#3599,.F.);
#5127=ORIENTED_EDGE('',*,*,#3628,.F.);
#5128=ORIENTED_EDGE('',*,*,#3597,.F.);
#5129=ORIENTED_EDGE('',*,*,#3626,.F.);
#5130=ORIENTED_EDGE('',*,*,#3623,.F.);
#5131=ORIENTED_EDGE('',*,*,#3621,.F.);
#5132=ORIENTED_EDGE('',*,*,#3619,.F.);
#5133=ORIENTED_EDGE('',*,*,#3617,.F.);
#5134=ORIENTED_EDGE('',*,*,#3615,.F.);
#5135=ORIENTED_EDGE('',*,*,#3613,.F.);
#5136=ORIENTED_EDGE('',*,*,#3610,.F.);
#5137=ORIENTED_EDGE('',*,*,#3607,.F.);
#5138=ORIENTED_EDGE('',*,*,#3604,.F.);
#5139=ORIENTED_EDGE('',*,*,#3601,.F.);
#5140=ORIENTED_EDGE('',*,*,#3536,.T.);
#5141=ORIENTED_EDGE('',*,*,#3539,.T.);
#5142=ORIENTED_EDGE('',*,*,#3542,.T.);
#5143=ORIENTED_EDGE('',*,*,#3545,.T.);
#5144=ORIENTED_EDGE('',*,*,#3579,.F.);
#5145=ORIENTED_EDGE('',*,*,#3628,.T.);
#5146=ORIENTED_EDGE('',*,*,#3603,.F.);
#5147=ORIENTED_EDGE('',*,*,#3629,.F.);
#5148=ORIENTED_EDGE('',*,*,#3576,.F.);
#5149=ORIENTED_EDGE('',*,*,#3629,.T.);
#5150=ORIENTED_EDGE('',*,*,#3606,.F.);
#5151=ORIENTED_EDGE('',*,*,#3630,.F.);
#5152=ORIENTED_EDGE('',*,*,#3571,.F.);
#5153=ORIENTED_EDGE('',*,*,#3630,.T.);
#5154=ORIENTED_EDGE('',*,*,#3609,.F.);
#5155=ORIENTED_EDGE('',*,*,#3631,.F.);
#5156=ORIENTED_EDGE('',*,*,#3568,.F.);
#5157=ORIENTED_EDGE('',*,*,#3631,.T.);
#5158=ORIENTED_EDGE('',*,*,#3612,.F.);
#5159=ORIENTED_EDGE('',*,*,#3595,.F.);
#5160=ORIENTED_EDGE('',*,*,#3632,.T.);
#5161=ORIENTED_EDGE('',*,*,#3633,.T.);
#5162=ORIENTED_EDGE('',*,*,#3634,.T.);
#5163=ORIENTED_EDGE('',*,*,#3635,.T.);
#5164=ORIENTED_EDGE('',*,*,#3636,.T.);
#5165=ORIENTED_EDGE('',*,*,#3637,.T.);
#5166=ORIENTED_EDGE('',*,*,#3638,.T.);
#5167=ORIENTED_EDGE('',*,*,#3639,.T.);
#5168=ORIENTED_EDGE('',*,*,#3640,.T.);
#5169=ORIENTED_EDGE('',*,*,#3641,.T.);
#5170=ORIENTED_EDGE('',*,*,#3642,.T.);
#5171=ORIENTED_EDGE('',*,*,#3637,.F.);
#5172=ORIENTED_EDGE('',*,*,#3643,.T.);
#5173=ORIENTED_EDGE('',*,*,#3644,.T.);
#5174=ORIENTED_EDGE('',*,*,#3645,.T.);
#5175=ORIENTED_EDGE('',*,*,#3641,.F.);
#5176=ORIENTED_EDGE('',*,*,#3646,.T.);
#5177=ORIENTED_EDGE('',*,*,#3647,.T.);
#5178=ORIENTED_EDGE('',*,*,#3648,.T.);
#5179=ORIENTED_EDGE('',*,*,#3644,.F.);
#5180=ORIENTED_EDGE('',*,*,#3649,.T.);
#5181=ORIENTED_EDGE('',*,*,#3650,.T.);
#5182=ORIENTED_EDGE('',*,*,#3651,.T.);
#5183=ORIENTED_EDGE('',*,*,#3647,.F.);
#5184=ORIENTED_EDGE('',*,*,#3652,.T.);
#5185=ORIENTED_EDGE('',*,*,#3650,.F.);
#5186=ORIENTED_EDGE('',*,*,#3653,.T.);
#5187=ORIENTED_EDGE('',*,*,#3654,.T.);
#5188=ORIENTED_EDGE('',*,*,#3655,.T.);
#5189=ORIENTED_EDGE('',*,*,#3654,.F.);
#5190=ORIENTED_EDGE('',*,*,#3656,.T.);
#5191=ORIENTED_EDGE('',*,*,#3657,.T.);
#5192=ORIENTED_EDGE('',*,*,#3658,.T.);
#5193=ORIENTED_EDGE('',*,*,#3657,.F.);
#5194=ORIENTED_EDGE('',*,*,#3659,.T.);
#5195=ORIENTED_EDGE('',*,*,#3660,.T.);
#5196=ORIENTED_EDGE('',*,*,#3661,.T.);
#5197=ORIENTED_EDGE('',*,*,#3660,.F.);
#5198=ORIENTED_EDGE('',*,*,#3662,.T.);
#5199=ORIENTED_EDGE('',*,*,#3663,.T.);
#5200=ORIENTED_EDGE('',*,*,#3664,.T.);
#5201=ORIENTED_EDGE('',*,*,#3663,.F.);
#5202=ORIENTED_EDGE('',*,*,#3665,.T.);
#5203=ORIENTED_EDGE('',*,*,#3633,.F.);
#5204=ORIENTED_EDGE('',*,*,#3666,.T.);
#5205=ORIENTED_EDGE('',*,*,#3635,.F.);
#5206=ORIENTED_EDGE('',*,*,#3667,.T.);
#5207=ORIENTED_EDGE('',*,*,#3639,.F.);
#5208=ORIENTED_EDGE('',*,*,#3658,.F.);
#5209=ORIENTED_EDGE('',*,*,#3668,.T.);
#5210=ORIENTED_EDGE('',*,*,#3669,.F.);
#5211=ORIENTED_EDGE('',*,*,#3670,.T.);
#5212=ORIENTED_EDGE('',*,*,#3661,.F.);
#5213=ORIENTED_EDGE('',*,*,#3671,.F.);
#5214=ORIENTED_EDGE('',*,*,#3672,.F.);
#5215=ORIENTED_EDGE('',*,*,#3668,.F.);
#5216=ORIENTED_EDGE('',*,*,#3664,.F.);
#5217=ORIENTED_EDGE('',*,*,#3673,.T.);
#5218=ORIENTED_EDGE('',*,*,#3674,.F.);
#5219=ORIENTED_EDGE('',*,*,#3671,.T.);
#5220=ORIENTED_EDGE('',*,*,#3632,.F.);
#5221=ORIENTED_EDGE('',*,*,#3675,.F.);
#5222=ORIENTED_EDGE('',*,*,#3676,.F.);
#5223=ORIENTED_EDGE('',*,*,#3673,.F.);
#5224=ORIENTED_EDGE('',*,*,#3666,.F.);
#5225=ORIENTED_EDGE('',*,*,#3677,.T.);
#5226=ORIENTED_EDGE('',*,*,#3678,.F.);
#5227=ORIENTED_EDGE('',*,*,#3675,.T.);
#5228=ORIENTED_EDGE('',*,*,#3638,.F.);
#5229=ORIENTED_EDGE('',*,*,#3679,.F.);
#5230=ORIENTED_EDGE('',*,*,#3680,.F.);
#5231=ORIENTED_EDGE('',*,*,#3677,.F.);
#5232=ORIENTED_EDGE('',*,*,#3636,.F.);
#5233=ORIENTED_EDGE('',*,*,#3667,.F.);
#5234=ORIENTED_EDGE('',*,*,#3634,.F.);
#5235=ORIENTED_EDGE('',*,*,#3665,.F.);
#5236=ORIENTED_EDGE('',*,*,#3662,.F.);
#5237=ORIENTED_EDGE('',*,*,#3659,.F.);
#5238=ORIENTED_EDGE('',*,*,#3656,.F.);
#5239=ORIENTED_EDGE('',*,*,#3653,.F.);
#5240=ORIENTED_EDGE('',*,*,#3649,.F.);
#5241=ORIENTED_EDGE('',*,*,#3646,.F.);
#5242=ORIENTED_EDGE('',*,*,#3643,.F.);
#5243=ORIENTED_EDGE('',*,*,#3640,.F.);
#5244=ORIENTED_EDGE('',*,*,#3681,.T.);
#5245=ORIENTED_EDGE('',*,*,#3682,.T.);
#5246=ORIENTED_EDGE('',*,*,#3676,.T.);
#5247=ORIENTED_EDGE('',*,*,#3683,.F.);
#5248=ORIENTED_EDGE('',*,*,#3684,.T.);
#5249=ORIENTED_EDGE('',*,*,#3685,.T.);
#5250=ORIENTED_EDGE('',*,*,#3674,.T.);
#5251=ORIENTED_EDGE('',*,*,#3682,.F.);
#5252=ORIENTED_EDGE('',*,*,#3686,.T.);
#5253=ORIENTED_EDGE('',*,*,#3687,.T.);
#5254=ORIENTED_EDGE('',*,*,#3672,.T.);
#5255=ORIENTED_EDGE('',*,*,#3685,.F.);
#5256=ORIENTED_EDGE('',*,*,#3688,.T.);
#5257=ORIENTED_EDGE('',*,*,#3689,.T.);
#5258=ORIENTED_EDGE('',*,*,#3669,.T.);
#5259=ORIENTED_EDGE('',*,*,#3687,.F.);
#5260=ORIENTED_EDGE('',*,*,#3690,.T.);
#5261=ORIENTED_EDGE('',*,*,#3691,.T.);
#5262=ORIENTED_EDGE('',*,*,#3692,.T.);
#5263=ORIENTED_EDGE('',*,*,#3689,.F.);
#5264=ORIENTED_EDGE('',*,*,#3693,.T.);
#5265=ORIENTED_EDGE('',*,*,#3691,.F.);
#5266=ORIENTED_EDGE('',*,*,#3694,.T.);
#5267=ORIENTED_EDGE('',*,*,#3695,.T.);
#5268=ORIENTED_EDGE('',*,*,#3696,.T.);
#5269=ORIENTED_EDGE('',*,*,#3695,.F.);
#5270=ORIENTED_EDGE('',*,*,#3697,.T.);
#5271=ORIENTED_EDGE('',*,*,#3698,.T.);
#5272=ORIENTED_EDGE('',*,*,#3699,.T.);
#5273=ORIENTED_EDGE('',*,*,#3698,.F.);
#5274=ORIENTED_EDGE('',*,*,#3700,.T.);
#5275=ORIENTED_EDGE('',*,*,#3701,.T.);
#5276=ORIENTED_EDGE('',*,*,#3702,.T.);
#5277=ORIENTED_EDGE('',*,*,#3701,.F.);
#5278=ORIENTED_EDGE('',*,*,#3703,.T.);
#5279=ORIENTED_EDGE('',*,*,#3704,.T.);
#5280=ORIENTED_EDGE('',*,*,#3705,.T.);
#5281=ORIENTED_EDGE('',*,*,#3704,.F.);
#5282=ORIENTED_EDGE('',*,*,#3706,.T.);
#5283=ORIENTED_EDGE('',*,*,#3707,.T.);
#5284=ORIENTED_EDGE('',*,*,#3680,.T.);
#5285=ORIENTED_EDGE('',*,*,#3707,.F.);
#5286=ORIENTED_EDGE('',*,*,#3708,.T.);
#5287=ORIENTED_EDGE('',*,*,#3709,.T.);
#5288=ORIENTED_EDGE('',*,*,#3678,.T.);
#5289=ORIENTED_EDGE('',*,*,#3709,.F.);
#5290=ORIENTED_EDGE('',*,*,#3710,.T.);
#5291=ORIENTED_EDGE('',*,*,#3683,.T.);
#5292=ORIENTED_EDGE('',*,*,#3648,.F.);
#5293=ORIENTED_EDGE('',*,*,#3711,.T.);
#5294=ORIENTED_EDGE('',*,*,#3699,.F.);
#5295=ORIENTED_EDGE('',*,*,#3712,.T.);
#5296=ORIENTED_EDGE('',*,*,#3645,.F.);
#5297=ORIENTED_EDGE('',*,*,#3712,.F.);
#5298=ORIENTED_EDGE('',*,*,#3702,.F.);
#5299=ORIENTED_EDGE('',*,*,#3713,.F.);
#5300=ORIENTED_EDGE('',*,*,#3642,.F.);
#5301=ORIENTED_EDGE('',*,*,#3713,.T.);
#5302=ORIENTED_EDGE('',*,*,#3705,.F.);
#5303=ORIENTED_EDGE('',*,*,#3679,.T.);
#5304=ORIENTED_EDGE('',*,*,#3681,.F.);
#5305=ORIENTED_EDGE('',*,*,#3710,.F.);
#5306=ORIENTED_EDGE('',*,*,#3708,.F.);
#5307=ORIENTED_EDGE('',*,*,#3706,.F.);
#5308=ORIENTED_EDGE('',*,*,#3703,.F.);
#5309=ORIENTED_EDGE('',*,*,#3700,.F.);
#5310=ORIENTED_EDGE('',*,*,#3697,.F.);
#5311=ORIENTED_EDGE('',*,*,#3694,.F.);
#5312=ORIENTED_EDGE('',*,*,#3690,.F.);
#5313=ORIENTED_EDGE('',*,*,#3688,.F.);
#5314=ORIENTED_EDGE('',*,*,#3686,.F.);
#5315=ORIENTED_EDGE('',*,*,#3684,.F.);
#5316=ORIENTED_EDGE('',*,*,#3652,.F.);
#5317=ORIENTED_EDGE('',*,*,#3714,.T.);
#5318=ORIENTED_EDGE('',*,*,#3693,.F.);
#5319=ORIENTED_EDGE('',*,*,#3715,.T.);
#5320=ORIENTED_EDGE('',*,*,#3651,.F.);
#5321=ORIENTED_EDGE('',*,*,#3715,.F.);
#5322=ORIENTED_EDGE('',*,*,#3696,.F.);
#5323=ORIENTED_EDGE('',*,*,#3711,.F.);
#5324=ORIENTED_EDGE('',*,*,#3655,.F.);
#5325=ORIENTED_EDGE('',*,*,#3670,.F.);
#5326=ORIENTED_EDGE('',*,*,#3692,.F.);
#5327=ORIENTED_EDGE('',*,*,#3714,.F.);
#5328=CYLINDRICAL_SURFACE('',#6002,10.);
#5329=CYLINDRICAL_SURFACE('',#6005,10.);
#5330=CYLINDRICAL_SURFACE('',#6008,10.);
#5331=CYLINDRICAL_SURFACE('',#6011,10.);
#5332=CYLINDRICAL_SURFACE('',#6014,10.);
#5333=CYLINDRICAL_SURFACE('',#6017,10.);
#5334=CYLINDRICAL_SURFACE('',#6020,10.);
#5335=CYLINDRICAL_SURFACE('',#6023,10.);
#5336=CYLINDRICAL_SURFACE('',#6026,10.);
#5337=CYLINDRICAL_SURFACE('',#6034,10.);
#5338=CYLINDRICAL_SURFACE('',#6037,10.);
#5339=CYLINDRICAL_SURFACE('',#6039,10.);
#5340=CYLINDRICAL_SURFACE('',#6045,3.);
#5341=CYLINDRICAL_SURFACE('',#6079,4.);
#5342=CYLINDRICAL_SURFACE('',#6089,4.);
#5343=CYLINDRICAL_SURFACE('',#6095,3.);
#5344=CYLINDRICAL_SURFACE('',#6098,3.);
#5345=CYLINDRICAL_SURFACE('',#6101,3.);
#5346=CYLINDRICAL_SURFACE('',#6104,3.);
#5347=CYLINDRICAL_SURFACE('',#6108,1.);
#5348=CYLINDRICAL_SURFACE('',#6110,1.);
#5349=CYLINDRICAL_SURFACE('',#6114,1.);
#5350=CYLINDRICAL_SURFACE('',#6116,1.);
#5351=CYLINDRICAL_SURFACE('',#6118,1.);
#5352=CYLINDRICAL_SURFACE('',#6121,1.);
#5353=CYLINDRICAL_SURFACE('',#6124,1.);
#5354=CYLINDRICAL_SURFACE('',#6126,1.);
#5355=CYLINDRICAL_SURFACE('',#6129,1.);
#5356=CYLINDRICAL_SURFACE('',#6131,1.);
#5357=CYLINDRICAL_SURFACE('',#6132,1.);
#5358=CYLINDRICAL_SURFACE('',#6134,1.);
#5359=CYLINDRICAL_SURFACE('',#6136,1.);
#5360=CYLINDRICAL_SURFACE('',#6137,1.);
#5361=CYLINDRICAL_SURFACE('',#6139,1.);
#5362=CYLINDRICAL_SURFACE('',#6141,1.);
#5363=CYLINDRICAL_SURFACE('',#6149,1.);
#5364=CYLINDRICAL_SURFACE('',#6151,1.);
#5365=CYLINDRICAL_SURFACE('',#6153,1.);
#5366=CYLINDRICAL_SURFACE('',#6154,1.);
#5367=CYLINDRICAL_SURFACE('',#6156,1.);
#5368=CYLINDRICAL_SURFACE('',#6158,1.);
#5369=CYLINDRICAL_SURFACE('',#6160,1.);
#5370=CYLINDRICAL_SURFACE('',#6162,1.);
#5371=CYLINDRICAL_SURFACE('',#6164,1.);
#5372=CYLINDRICAL_SURFACE('',#6166,1.);
#5373=CYLINDRICAL_SURFACE('',#6174,1.);
#5374=CYLINDRICAL_SURFACE('',#6177,1.);
#5375=CYLINDRICAL_SURFACE('',#6180,1.);
#5376=CYLINDRICAL_SURFACE('',#6182,1.);
#5377=CYLINDRICAL_SURFACE('',#6184,1.);
#5378=CYLINDRICAL_SURFACE('',#6186,1.);
#5379=CYLINDRICAL_SURFACE('',#6188,1.);
#5380=CYLINDRICAL_SURFACE('',#6190,1.);
#5381=CYLINDRICAL_SURFACE('',#6192,1.);
#5382=CYLINDRICAL_SURFACE('',#6194,1.);
#5383=CYLINDRICAL_SURFACE('',#6196,1.);
#5384=CYLINDRICAL_SURFACE('',#6197,1.);
#5385=CYLINDRICAL_SURFACE('',#6205,1.);
#5386=CYLINDRICAL_SURFACE('',#6208,1.);
#5387=CYLINDRICAL_SURFACE('',#6210,1.);
#5388=CYLINDRICAL_SURFACE('',#6212,1.);
#5389=CYLINDRICAL_SURFACE('',#6214,1.);
#5390=CYLINDRICAL_SURFACE('',#6216,1.);
#5391=CYLINDRICAL_SURFACE('',#6218,1.);
#5392=CYLINDRICAL_SURFACE('',#6220,1.);
#5393=CYLINDRICAL_SURFACE('',#6222,1.);
#5394=CYLINDRICAL_SURFACE('',#6224,1.);
#5395=CYLINDRICAL_SURFACE('',#6226,1.);
#5396=CYLINDRICAL_SURFACE('',#6228,1.);
#5397=CYLINDRICAL_SURFACE('',#6237,3.00000000000001);
#5398=CYLINDRICAL_SURFACE('',#6240,3.);
#5399=CYLINDRICAL_SURFACE('',#6243,2.99999999999999);
#5400=CYLINDRICAL_SURFACE('',#6246,3.);
#5401=CYLINDRICAL_SURFACE('',#6249,3.);
#5402=CYLINDRICAL_SURFACE('',#6252,2.99999999999999);
#5403=CYLINDRICAL_SURFACE('',#6255,2.99999999999999);
#5404=CYLINDRICAL_SURFACE('',#6258,3.);
#5405=CYLINDRICAL_SURFACE('',#6261,3.);
#5406=CYLINDRICAL_SURFACE('',#6264,2.99999999999999);
#5407=CYLINDRICAL_SURFACE('',#6267,1.);
#5408=CYLINDRICAL_SURFACE('',#6270,1.);
#5409=CYLINDRICAL_SURFACE('',#6272,1.);
#5410=CYLINDRICAL_SURFACE('',#6274,1.);
#5411=CYLINDRICAL_SURFACE('',#6276,1.);
#5412=CYLINDRICAL_SURFACE('',#6278,1.);
#5413=CYLINDRICAL_SURFACE('',#6280,1.);
#5414=CYLINDRICAL_SURFACE('',#6282,1.);
#5415=CYLINDRICAL_SURFACE('',#6288,1.);
#5416=CYLINDRICAL_SURFACE('',#6291,1.);
#5417=CYLINDRICAL_SURFACE('',#6293,1.);
#5418=CYLINDRICAL_SURFACE('',#6295,1.);
#5419=CYLINDRICAL_SURFACE('',#6297,1.);
#5420=CYLINDRICAL_SURFACE('',#6299,1.);
#5421=CYLINDRICAL_SURFACE('',#6301,1.);
#5422=CYLINDRICAL_SURFACE('',#6303,1.);
#5423=CYLINDRICAL_SURFACE('',#6310,3.00000000000001);
#5424=CYLINDRICAL_SURFACE('',#6313,3.);
#5425=CYLINDRICAL_SURFACE('',#6327,3.);
#5426=CYLINDRICAL_SURFACE('',#6331,3.);
#5427=CYLINDRICAL_SURFACE('',#6335,3.);
#5428=CYLINDRICAL_SURFACE('',#6339,2.);
#5429=CYLINDRICAL_SURFACE('',#6342,2.);
#5430=CYLINDRICAL_SURFACE('',#6344,2.);
#5431=CYLINDRICAL_SURFACE('',#6346,2.);
#5432=CYLINDRICAL_SURFACE('',#6356,1.);
#5433=CYLINDRICAL_SURFACE('',#6358,1.);
#5434=CYLINDRICAL_SURFACE('',#6361,1.);
#5435=CYLINDRICAL_SURFACE('',#6363,1.);
#5436=CYLINDRICAL_SURFACE('',#6366,1.);
#5437=CYLINDRICAL_SURFACE('',#6368,1.);
#5438=CYLINDRICAL_SURFACE('',#6370,1.);
#5439=CYLINDRICAL_SURFACE('',#6372,1.);
#5440=CYLINDRICAL_SURFACE('',#6374,1.);
#5441=CYLINDRICAL_SURFACE('',#6375,1.);
#5442=CYLINDRICAL_SURFACE('',#6380,1.);
#5443=CYLINDRICAL_SURFACE('',#6383,1.);
#5444=CYLINDRICAL_SURFACE('',#6385,1.);
#5445=CYLINDRICAL_SURFACE('',#6387,1.);
#5446=CYLINDRICAL_SURFACE('',#6389,1.);
#5447=CYLINDRICAL_SURFACE('',#6391,1.);
#5448=CYLINDRICAL_SURFACE('',#6393,1.);
#5449=CYLINDRICAL_SURFACE('',#6394,1.);
#5450=CYLINDRICAL_SURFACE('',#6400,3.);
#5451=CYLINDRICAL_SURFACE('',#6403,3.);
#5452=CYLINDRICAL_SURFACE('',#6406,3.);
#5453=CYLINDRICAL_SURFACE('',#6409,3.);
#5454=CYLINDRICAL_SURFACE('',#6412,1.);
#5455=CYLINDRICAL_SURFACE('',#6415,1.);
#5456=CYLINDRICAL_SURFACE('',#6418,1.);
#5457=CYLINDRICAL_SURFACE('',#6420,1.);
#5458=CYLINDRICAL_SURFACE('',#6423,1.);
#5459=CYLINDRICAL_SURFACE('',#6425,1.);
#5460=CYLINDRICAL_SURFACE('',#6426,1.);
#5461=CYLINDRICAL_SURFACE('',#6428,1.);
#5462=CYLINDRICAL_SURFACE('',#6430,1.);
#5463=CYLINDRICAL_SURFACE('',#6431,1.);
#5464=CYLINDRICAL_SURFACE('',#6433,1.);
#5465=CYLINDRICAL_SURFACE('',#6435,1.);
#5466=CYLINDRICAL_SURFACE('',#6443,1.);
#5467=CYLINDRICAL_SURFACE('',#6446,1.);
#5468=CYLINDRICAL_SURFACE('',#6448,1.);
#5469=CYLINDRICAL_SURFACE('',#6450,1.);
#5470=CYLINDRICAL_SURFACE('',#6452,1.);
#5471=CYLINDRICAL_SURFACE('',#6454,1.);
#5472=CYLINDRICAL_SURFACE('',#6456,1.);
#5473=CYLINDRICAL_SURFACE('',#6458,1.);
#5474=CYLINDRICAL_SURFACE('',#6460,1.);
#5475=CYLINDRICAL_SURFACE('',#6462,1.);
#5476=CYLINDRICAL_SURFACE('',#6464,1.);
#5477=CYLINDRICAL_SURFACE('',#6466,1.);
#5478=CYLINDRICAL_SURFACE('',#6475,3.);
#5479=CYLINDRICAL_SURFACE('',#6478,3.);
#5480=CYLINDRICAL_SURFACE('',#6481,3.);
#5481=CYLINDRICAL_SURFACE('',#6484,3.);
#5482=CYLINDRICAL_SURFACE('',#6487,1.);
#5483=CYLINDRICAL_SURFACE('',#6490,1.);
#5484=CYLINDRICAL_SURFACE('',#6493,1.);
#5485=CYLINDRICAL_SURFACE('',#6495,1.);
#5486=CYLINDRICAL_SURFACE('',#6498,1.);
#5487=CYLINDRICAL_SURFACE('',#6500,1.);
#5488=CYLINDRICAL_SURFACE('',#6501,1.);
#5489=CYLINDRICAL_SURFACE('',#6503,1.);
#5490=CYLINDRICAL_SURFACE('',#6505,1.);
#5491=CYLINDRICAL_SURFACE('',#6506,1.);
#5492=CYLINDRICAL_SURFACE('',#6508,1.);
#5493=CYLINDRICAL_SURFACE('',#6510,1.);
#5494=CYLINDRICAL_SURFACE('',#6518,1.);
#5495=CYLINDRICAL_SURFACE('',#6521,1.);
#5496=CYLINDRICAL_SURFACE('',#6523,1.);
#5497=CYLINDRICAL_SURFACE('',#6525,1.);
#5498=CYLINDRICAL_SURFACE('',#6527,1.);
#5499=CYLINDRICAL_SURFACE('',#6529,1.);
#5500=CYLINDRICAL_SURFACE('',#6531,1.);
#5501=CYLINDRICAL_SURFACE('',#6533,1.);
#5502=CYLINDRICAL_SURFACE('',#6535,1.);
#5503=CYLINDRICAL_SURFACE('',#6537,1.);
#5504=CYLINDRICAL_SURFACE('',#6539,1.);
#5505=CYLINDRICAL_SURFACE('',#6541,1.);
#5506=CYLINDRICAL_SURFACE('',#6550,1.);
#5507=CYLINDRICAL_SURFACE('',#6553,1.);
#5508=CYLINDRICAL_SURFACE('',#6556,1.);
#5509=CYLINDRICAL_SURFACE('',#6558,1.);
#5510=CYLINDRICAL_SURFACE('',#6560,1.);
#5511=CYLINDRICAL_SURFACE('',#6562,1.);
#5512=CYLINDRICAL_SURFACE('',#6564,1.);
#5513=CYLINDRICAL_SURFACE('',#6566,1.);
#5514=CYLINDRICAL_SURFACE('',#6568,1.);
#5515=CYLINDRICAL_SURFACE('',#6570,1.);
#5516=CYLINDRICAL_SURFACE('',#6572,1.);
#5517=CYLINDRICAL_SURFACE('',#6573,1.);
#5518=CYLINDRICAL_SURFACE('',#6581,1.);
#5519=CYLINDRICAL_SURFACE('',#6584,1.);
#5520=CYLINDRICAL_SURFACE('',#6586,1.);
#5521=CYLINDRICAL_SURFACE('',#6588,1.);
#5522=CYLINDRICAL_SURFACE('',#6590,1.);
#5523=CYLINDRICAL_SURFACE('',#6592,1.);
#5524=CYLINDRICAL_SURFACE('',#6594,1.);
#5525=CYLINDRICAL_SURFACE('',#6596,1.);
#5526=CYLINDRICAL_SURFACE('',#6598,1.);
#5527=CYLINDRICAL_SURFACE('',#6600,1.);
#5528=CYLINDRICAL_SURFACE('',#6602,1.);
#5529=CYLINDRICAL_SURFACE('',#6604,1.);
#5530=ADVANCED_FACE('',(#467),#5328,.F.);
#5531=ADVANCED_FACE('',(#468),#5329,.F.);
#5532=ADVANCED_FACE('',(#469),#5330,.F.);
#5533=ADVANCED_FACE('',(#470),#5331,.F.);
#5534=ADVANCED_FACE('',(#471),#5332,.F.);
#5535=ADVANCED_FACE('',(#472),#5333,.F.);
#5536=ADVANCED_FACE('',(#473),#5334,.F.);
#5537=ADVANCED_FACE('',(#474),#5335,.F.);
#5538=ADVANCED_FACE('',(#475),#5336,.T.);
#5539=ADVANCED_FACE('',(#476),#324,.T.);
#5540=ADVANCED_FACE('',(#477,#255,#256,#257,#258,#259,#260,#261,#262),#325,
 .F.);
#5541=ADVANCED_FACE('',(#478),#5337,.T.);
#5542=ADVANCED_FACE('',(#479),#326,.T.);
#5543=ADVANCED_FACE('',(#480),#5338,.T.);
#5544=ADVANCED_FACE('',(#481),#5339,.T.);
#5545=ADVANCED_FACE('',(#482),#327,.T.);
#5546=ADVANCED_FACE('',(#483),#328,.T.);
#5547=ADVANCED_FACE('',(#484,#263,#264,#265,#266,#267,#268,#269,#270),#329,
 .T.);
#5548=ADVANCED_FACE('',(#485),#5340,.F.);
#5549=ADVANCED_FACE('',(#486),#330,.T.);
#5550=ADVANCED_FACE('',(#487),#331,.T.);
#5551=ADVANCED_FACE('',(#488),#332,.T.);
#5552=ADVANCED_FACE('',(#489),#333,.T.);
#5553=ADVANCED_FACE('',(#490),#334,.T.);
#5554=ADVANCED_FACE('',(#491),#335,.T.);
#5555=ADVANCED_FACE('',(#492),#336,.T.);
#5556=ADVANCED_FACE('',(#493),#337,.T.);
#5557=ADVANCED_FACE('',(#494),#338,.T.);
#5558=ADVANCED_FACE('',(#495),#339,.T.);
#5559=ADVANCED_FACE('',(#496),#340,.T.);
#5560=ADVANCED_FACE('',(#497),#341,.T.);
#5561=ADVANCED_FACE('',(#498),#342,.T.);
#5562=ADVANCED_FACE('',(#499),#343,.T.);
#5563=ADVANCED_FACE('',(#500),#344,.T.);
#5564=ADVANCED_FACE('',(#501),#345,.T.);
#5565=ADVANCED_FACE('',(#502),#346,.T.);
#5566=ADVANCED_FACE('',(#503),#347,.T.);
#5567=ADVANCED_FACE('',(#504,#271),#348,.T.);
#5568=ADVANCED_FACE('',(#505),#349,.T.);
#5569=ADVANCED_FACE('',(#506),#350,.T.);
#5570=ADVANCED_FACE('',(#507,#272),#351,.F.);
#5571=ADVANCED_FACE('',(#508),#352,.T.);
#5572=ADVANCED_FACE('',(#509),#353,.T.);
#5573=ADVANCED_FACE('',(#510),#354,.T.);
#5574=ADVANCED_FACE('',(#511),#355,.T.);
#5575=ADVANCED_FACE('',(#512),#211,.F.);
#5576=ADVANCED_FACE('',(#513),#5341,.F.);
#5577=ADVANCED_FACE('',(#514),#212,.F.);
#5578=ADVANCED_FACE('',(#515),#356,.T.);
#5579=ADVANCED_FACE('',(#516),#213,.F.);
#5580=ADVANCED_FACE('',(#517),#5342,.F.);
#5581=ADVANCED_FACE('',(#518),#214,.F.);
#5582=ADVANCED_FACE('',(#519),#357,.T.);
#5583=ADVANCED_FACE('',(#520),#5343,.F.);
#5584=ADVANCED_FACE('',(#521),#5344,.F.);
#5585=ADVANCED_FACE('',(#522),#5345,.F.);
#5586=ADVANCED_FACE('',(#523),#5346,.F.);
#5587=ADVANCED_FACE('',(#524),#358,.T.);
#5588=ADVANCED_FACE('',(#525),#5347,.T.);
#5589=ADVANCED_FACE('',(#526),#5348,.T.);
#5590=ADVANCED_FACE('',(#527,#273,#274),#359,.T.);
#5591=ADVANCED_FACE('',(#528,#275,#276),#360,.T.);
#5592=ADVANCED_FACE('',(#529),#5349,.T.);
#5593=ADVANCED_FACE('',(#530),#5350,.T.);
#5594=ADVANCED_FACE('',(#531),#5351,.T.);
#5595=ADVANCED_FACE('',(#532),#5352,.T.);
#5596=ADVANCED_FACE('',(#533),#5353,.T.);
#5597=ADVANCED_FACE('',(#534),#5354,.T.);
#5598=ADVANCED_FACE('',(#535),#5355,.T.);
#5599=ADVANCED_FACE('',(#536),#5356,.T.);
#5600=ADVANCED_FACE('',(#537),#5357,.T.);
#5601=ADVANCED_FACE('',(#538),#5358,.T.);
#5602=ADVANCED_FACE('',(#539),#5359,.T.);
#5603=ADVANCED_FACE('',(#540),#5360,.T.);
#5604=ADVANCED_FACE('',(#541),#5361,.T.);
#5605=ADVANCED_FACE('',(#542),#5362,.T.);
#5606=ADVANCED_FACE('',(#543),#361,.T.);
#5607=ADVANCED_FACE('',(#544),#362,.T.);
#5608=ADVANCED_FACE('',(#545),#363,.T.);
#5609=ADVANCED_FACE('',(#546),#364,.T.);
#5610=ADVANCED_FACE('',(#547),#365,.T.);
#5611=ADVANCED_FACE('',(#548),#366,.T.);
#5612=ADVANCED_FACE('',(#549,#277,#278,#279,#280),#367,.F.);
#5613=ADVANCED_FACE('',(#550),#5363,.T.);
#5614=ADVANCED_FACE('',(#551),#5364,.T.);
#5615=ADVANCED_FACE('',(#552),#5365,.T.);
#5616=ADVANCED_FACE('',(#553),#5366,.T.);
#5617=ADVANCED_FACE('',(#554),#5367,.T.);
#5618=ADVANCED_FACE('',(#555),#5368,.T.);
#5619=ADVANCED_FACE('',(#556),#5369,.T.);
#5620=ADVANCED_FACE('',(#557),#5370,.T.);
#5621=ADVANCED_FACE('',(#558),#5371,.T.);
#5622=ADVANCED_FACE('',(#559),#5372,.T.);
#5623=ADVANCED_FACE('',(#560),#368,.T.);
#5624=ADVANCED_FACE('',(#561),#369,.T.);
#5625=ADVANCED_FACE('',(#562),#370,.T.);
#5626=ADVANCED_FACE('',(#563),#371,.T.);
#5627=ADVANCED_FACE('',(#564),#372,.T.);
#5628=ADVANCED_FACE('',(#565),#373,.T.);
#5629=ADVANCED_FACE('',(#566),#5373,.T.);
#5630=ADVANCED_FACE('',(#567),#5374,.T.);
#5631=ADVANCED_FACE('',(#568),#5375,.T.);
#5632=ADVANCED_FACE('',(#569),#5376,.T.);
#5633=ADVANCED_FACE('',(#570),#5377,.T.);
#5634=ADVANCED_FACE('',(#571),#5378,.T.);
#5635=ADVANCED_FACE('',(#572),#5379,.T.);
#5636=ADVANCED_FACE('',(#573),#5380,.T.);
#5637=ADVANCED_FACE('',(#574),#5381,.T.);
#5638=ADVANCED_FACE('',(#575),#5382,.T.);
#5639=ADVANCED_FACE('',(#576),#5383,.T.);
#5640=ADVANCED_FACE('',(#577),#5384,.T.);
#5641=ADVANCED_FACE('',(#578),#374,.T.);
#5642=ADVANCED_FACE('',(#579),#375,.T.);
#5643=ADVANCED_FACE('',(#580),#376,.T.);
#5644=ADVANCED_FACE('',(#581),#377,.T.);
#5645=ADVANCED_FACE('',(#582),#378,.T.);
#5646=ADVANCED_FACE('',(#583),#379,.T.);
#5647=ADVANCED_FACE('',(#584),#380,.F.);
#5648=ADVANCED_FACE('',(#585),#5385,.T.);
#5649=ADVANCED_FACE('',(#586),#5386,.T.);
#5650=ADVANCED_FACE('',(#587),#5387,.T.);
#5651=ADVANCED_FACE('',(#588),#5388,.T.);
#5652=ADVANCED_FACE('',(#589),#5389,.T.);
#5653=ADVANCED_FACE('',(#590),#5390,.T.);
#5654=ADVANCED_FACE('',(#591),#5391,.T.);
#5655=ADVANCED_FACE('',(#592),#5392,.T.);
#5656=ADVANCED_FACE('',(#593),#5393,.T.);
#5657=ADVANCED_FACE('',(#594),#5394,.T.);
#5658=ADVANCED_FACE('',(#595),#5395,.T.);
#5659=ADVANCED_FACE('',(#596),#5396,.T.);
#5660=ADVANCED_FACE('',(#597),#381,.T.);
#5661=ADVANCED_FACE('',(#598),#382,.T.);
#5662=ADVANCED_FACE('',(#599),#383,.T.);
#5663=ADVANCED_FACE('',(#600),#384,.T.);
#5664=ADVANCED_FACE('',(#601),#385,.T.);
#5665=ADVANCED_FACE('',(#602),#386,.T.);
#5666=ADVANCED_FACE('',(#603),#387,.T.);
#5667=ADVANCED_FACE('',(#604),#5397,.F.);
#5668=ADVANCED_FACE('',(#605),#5398,.F.);
#5669=ADVANCED_FACE('',(#606),#5399,.F.);
#5670=ADVANCED_FACE('',(#607),#5400,.F.);
#5671=ADVANCED_FACE('',(#608),#5401,.F.);
#5672=ADVANCED_FACE('',(#609),#5402,.F.);
#5673=ADVANCED_FACE('',(#610),#5403,.F.);
#5674=ADVANCED_FACE('',(#611),#5404,.F.);
#5675=ADVANCED_FACE('',(#612),#5405,.F.);
#5676=ADVANCED_FACE('',(#613),#5406,.F.);
#5677=ADVANCED_FACE('',(#614),#5407,.T.);
#5678=ADVANCED_FACE('',(#615),#5408,.T.);
#5679=ADVANCED_FACE('',(#616),#5409,.T.);
#5680=ADVANCED_FACE('',(#617),#5410,.T.);
#5681=ADVANCED_FACE('',(#618),#5411,.T.);
#5682=ADVANCED_FACE('',(#619),#5412,.T.);
#5683=ADVANCED_FACE('',(#620),#5413,.T.);
#5684=ADVANCED_FACE('',(#621),#5414,.T.);
#5685=ADVANCED_FACE('',(#622),#388,.T.);
#5686=ADVANCED_FACE('',(#623),#389,.T.);
#5687=ADVANCED_FACE('',(#624),#390,.T.);
#5688=ADVANCED_FACE('',(#625),#391,.T.);
#5689=ADVANCED_FACE('',(#626,#281,#282,#283,#284,#285,#286,#287,#288,#289,
#290),#392,.F.);
#5690=ADVANCED_FACE('',(#627),#5415,.T.);
#5691=ADVANCED_FACE('',(#628),#5416,.T.);
#5692=ADVANCED_FACE('',(#629),#5417,.T.);
#5693=ADVANCED_FACE('',(#630),#5418,.T.);
#5694=ADVANCED_FACE('',(#631),#5419,.T.);
#5695=ADVANCED_FACE('',(#632),#5420,.T.);
#5696=ADVANCED_FACE('',(#633),#5421,.T.);
#5697=ADVANCED_FACE('',(#634),#5422,.T.);
#5698=ADVANCED_FACE('',(#635),#393,.T.);
#5699=ADVANCED_FACE('',(#636),#394,.T.);
#5700=ADVANCED_FACE('',(#637),#395,.T.);
#5701=ADVANCED_FACE('',(#638,#291,#292,#293,#294,#295,#296,#297,#298,#299,
#300),#396,.T.);
#5702=ADVANCED_FACE('',(#639),#397,.T.);
#5703=ADVANCED_FACE('',(#640),#5423,.F.);
#5704=ADVANCED_FACE('',(#641),#5424,.F.);
#5705=ADVANCED_FACE('',(#642),#398,.T.);
#5706=ADVANCED_FACE('',(#643),#399,.T.);
#5707=ADVANCED_FACE('',(#644,#301),#400,.T.);
#5708=ADVANCED_FACE('',(#645),#401,.T.);
#5709=ADVANCED_FACE('',(#646,#302,#303),#402,.T.);
#5710=ADVANCED_FACE('',(#647),#403,.T.);
#5711=ADVANCED_FACE('',(#648,#304),#404,.T.);
#5712=ADVANCED_FACE('',(#649),#405,.T.);
#5713=ADVANCED_FACE('',(#650),#406,.T.);
#5714=ADVANCED_FACE('',(#651),#407,.T.);
#5715=ADVANCED_FACE('',(#652),#5425,.F.);
#5716=ADVANCED_FACE('',(#653),#408,.T.);
#5717=ADVANCED_FACE('',(#654),#5426,.F.);
#5718=ADVANCED_FACE('',(#655),#409,.T.);
#5719=ADVANCED_FACE('',(#656),#5427,.F.);
#5720=ADVANCED_FACE('',(#657),#410,.T.);
#5721=ADVANCED_FACE('',(#658),#5428,.T.);
#5722=ADVANCED_FACE('',(#659),#5429,.T.);
#5723=ADVANCED_FACE('',(#660),#5430,.T.);
#5724=ADVANCED_FACE('',(#661),#5431,.T.);
#5725=ADVANCED_FACE('',(#662),#411,.T.);
#5726=ADVANCED_FACE('',(#663),#412,.T.);
#5727=ADVANCED_FACE('',(#664,#305,#306,#307),#413,.T.);
#5728=ADVANCED_FACE('',(#665),#414,.T.);
#5729=ADVANCED_FACE('',(#666),#415,.F.);
#5730=ADVANCED_FACE('',(#667),#5432,.T.);
#5731=ADVANCED_FACE('',(#668),#5433,.T.);
#5732=ADVANCED_FACE('',(#669),#416,.T.);
#5733=ADVANCED_FACE('',(#670),#5434,.T.);
#5734=ADVANCED_FACE('',(#671),#5435,.T.);
#5735=ADVANCED_FACE('',(#672),#5436,.T.);
#5736=ADVANCED_FACE('',(#673),#5437,.T.);
#5737=ADVANCED_FACE('',(#674),#5438,.T.);
#5738=ADVANCED_FACE('',(#675),#5439,.T.);
#5739=ADVANCED_FACE('',(#676),#5440,.T.);
#5740=ADVANCED_FACE('',(#677),#5441,.T.);
#5741=ADVANCED_FACE('',(#678),#417,.T.);
#5742=ADVANCED_FACE('',(#679),#418,.T.);
#5743=ADVANCED_FACE('',(#680),#419,.T.);
#5744=ADVANCED_FACE('',(#681),#420,.T.);
#5745=ADVANCED_FACE('',(#682),#5442,.T.);
#5746=ADVANCED_FACE('',(#683),#5443,.T.);
#5747=ADVANCED_FACE('',(#684),#5444,.T.);
#5748=ADVANCED_FACE('',(#685),#5445,.T.);
#5749=ADVANCED_FACE('',(#686),#5446,.T.);
#5750=ADVANCED_FACE('',(#687),#5447,.T.);
#5751=ADVANCED_FACE('',(#688),#5448,.T.);
#5752=ADVANCED_FACE('',(#689),#5449,.T.);
#5753=ADVANCED_FACE('',(#690),#421,.T.);
#5754=ADVANCED_FACE('',(#691),#422,.T.);
#5755=ADVANCED_FACE('',(#692),#423,.T.);
#5756=ADVANCED_FACE('',(#693),#424,.T.);
#5757=ADVANCED_FACE('',(#694),#5450,.F.);
#5758=ADVANCED_FACE('',(#695),#5451,.F.);
#5759=ADVANCED_FACE('',(#696),#5452,.F.);
#5760=ADVANCED_FACE('',(#697),#5453,.F.);
#5761=ADVANCED_FACE('',(#698),#5454,.T.);
#5762=ADVANCED_FACE('',(#699),#5455,.T.);
#5763=ADVANCED_FACE('',(#700),#5456,.T.);
#5764=ADVANCED_FACE('',(#701),#5457,.T.);
#5765=ADVANCED_FACE('',(#702),#5458,.T.);
#5766=ADVANCED_FACE('',(#703),#5459,.T.);
#5767=ADVANCED_FACE('',(#704),#5460,.T.);
#5768=ADVANCED_FACE('',(#705),#5461,.T.);
#5769=ADVANCED_FACE('',(#706),#5462,.T.);
#5770=ADVANCED_FACE('',(#707),#5463,.T.);
#5771=ADVANCED_FACE('',(#708),#5464,.T.);
#5772=ADVANCED_FACE('',(#709),#5465,.T.);
#5773=ADVANCED_FACE('',(#710),#425,.T.);
#5774=ADVANCED_FACE('',(#711),#426,.T.);
#5775=ADVANCED_FACE('',(#712),#427,.T.);
#5776=ADVANCED_FACE('',(#713),#428,.T.);
#5777=ADVANCED_FACE('',(#714),#429,.T.);
#5778=ADVANCED_FACE('',(#715),#430,.T.);
#5779=ADVANCED_FACE('',(#716,#308,#309,#310,#311),#431,.F.);
#5780=ADVANCED_FACE('',(#717),#5466,.T.);
#5781=ADVANCED_FACE('',(#718),#5467,.T.);
#5782=ADVANCED_FACE('',(#719),#5468,.T.);
#5783=ADVANCED_FACE('',(#720),#5469,.T.);
#5784=ADVANCED_FACE('',(#721),#5470,.T.);
#5785=ADVANCED_FACE('',(#722),#5471,.T.);
#5786=ADVANCED_FACE('',(#723),#5472,.T.);
#5787=ADVANCED_FACE('',(#724),#5473,.T.);
#5788=ADVANCED_FACE('',(#725),#5474,.T.);
#5789=ADVANCED_FACE('',(#726),#5475,.T.);
#5790=ADVANCED_FACE('',(#727),#5476,.T.);
#5791=ADVANCED_FACE('',(#728),#5477,.T.);
#5792=ADVANCED_FACE('',(#729),#432,.T.);
#5793=ADVANCED_FACE('',(#730),#433,.T.);
#5794=ADVANCED_FACE('',(#731,#312,#313,#314,#315),#434,.T.);
#5795=ADVANCED_FACE('',(#732),#435,.T.);
#5796=ADVANCED_FACE('',(#733),#436,.T.);
#5797=ADVANCED_FACE('',(#734),#437,.T.);
#5798=ADVANCED_FACE('',(#735),#438,.T.);
#5799=ADVANCED_FACE('',(#736),#5478,.F.);
#5800=ADVANCED_FACE('',(#737),#5479,.F.);
#5801=ADVANCED_FACE('',(#738),#5480,.F.);
#5802=ADVANCED_FACE('',(#739),#5481,.F.);
#5803=ADVANCED_FACE('',(#740),#5482,.T.);
#5804=ADVANCED_FACE('',(#741),#5483,.T.);
#5805=ADVANCED_FACE('',(#742),#5484,.T.);
#5806=ADVANCED_FACE('',(#743),#5485,.T.);
#5807=ADVANCED_FACE('',(#744),#5486,.T.);
#5808=ADVANCED_FACE('',(#745),#5487,.T.);
#5809=ADVANCED_FACE('',(#746),#5488,.T.);
#5810=ADVANCED_FACE('',(#747),#5489,.T.);
#5811=ADVANCED_FACE('',(#748),#5490,.T.);
#5812=ADVANCED_FACE('',(#749),#5491,.T.);
#5813=ADVANCED_FACE('',(#750),#5492,.T.);
#5814=ADVANCED_FACE('',(#751),#5493,.T.);
#5815=ADVANCED_FACE('',(#752),#439,.T.);
#5816=ADVANCED_FACE('',(#753),#440,.T.);
#5817=ADVANCED_FACE('',(#754),#441,.T.);
#5818=ADVANCED_FACE('',(#755),#442,.T.);
#5819=ADVANCED_FACE('',(#756),#443,.T.);
#5820=ADVANCED_FACE('',(#757),#444,.T.);
#5821=ADVANCED_FACE('',(#758,#316,#317,#318,#319),#445,.F.);
#5822=ADVANCED_FACE('',(#759),#5494,.T.);
#5823=ADVANCED_FACE('',(#760),#5495,.T.);
#5824=ADVANCED_FACE('',(#761),#5496,.T.);
#5825=ADVANCED_FACE('',(#762),#5497,.T.);
#5826=ADVANCED_FACE('',(#763),#5498,.T.);
#5827=ADVANCED_FACE('',(#764),#5499,.T.);
#5828=ADVANCED_FACE('',(#765),#5500,.T.);
#5829=ADVANCED_FACE('',(#766),#5501,.T.);
#5830=ADVANCED_FACE('',(#767),#5502,.T.);
#5831=ADVANCED_FACE('',(#768),#5503,.T.);
#5832=ADVANCED_FACE('',(#769),#5504,.T.);
#5833=ADVANCED_FACE('',(#770),#5505,.T.);
#5834=ADVANCED_FACE('',(#771),#446,.T.);
#5835=ADVANCED_FACE('',(#772),#447,.T.);
#5836=ADVANCED_FACE('',(#773,#320,#321,#322,#323),#448,.T.);
#5837=ADVANCED_FACE('',(#774),#449,.T.);
#5838=ADVANCED_FACE('',(#775),#450,.T.);
#5839=ADVANCED_FACE('',(#776),#451,.T.);
#5840=ADVANCED_FACE('',(#777),#452,.T.);
#5841=ADVANCED_FACE('',(#778),#5506,.T.);
#5842=ADVANCED_FACE('',(#779),#5507,.T.);
#5843=ADVANCED_FACE('',(#780),#5508,.T.);
#5844=ADVANCED_FACE('',(#781),#5509,.T.);
#5845=ADVANCED_FACE('',(#782),#5510,.T.);
#5846=ADVANCED_FACE('',(#783),#5511,.T.);
#5847=ADVANCED_FACE('',(#784),#5512,.T.);
#5848=ADVANCED_FACE('',(#785),#5513,.T.);
#5849=ADVANCED_FACE('',(#786),#5514,.T.);
#5850=ADVANCED_FACE('',(#787),#5515,.T.);
#5851=ADVANCED_FACE('',(#788),#5516,.T.);
#5852=ADVANCED_FACE('',(#789),#5517,.T.);
#5853=ADVANCED_FACE('',(#790),#453,.T.);
#5854=ADVANCED_FACE('',(#791),#454,.T.);
#5855=ADVANCED_FACE('',(#792),#455,.T.);
#5856=ADVANCED_FACE('',(#793),#456,.T.);
#5857=ADVANCED_FACE('',(#794),#457,.T.);
#5858=ADVANCED_FACE('',(#795),#458,.T.);
#5859=ADVANCED_FACE('',(#796),#459,.F.);
#5860=ADVANCED_FACE('',(#797),#5518,.T.);
#5861=ADVANCED_FACE('',(#798),#5519,.T.);
#5862=ADVANCED_FACE('',(#799),#5520,.T.);
#5863=ADVANCED_FACE('',(#800),#5521,.T.);
#5864=ADVANCED_FACE('',(#801),#5522,.T.);
#5865=ADVANCED_FACE('',(#802),#5523,.T.);
#5866=ADVANCED_FACE('',(#803),#5524,.T.);
#5867=ADVANCED_FACE('',(#804),#5525,.T.);
#5868=ADVANCED_FACE('',(#805),#5526,.T.);
#5869=ADVANCED_FACE('',(#806),#5527,.T.);
#5870=ADVANCED_FACE('',(#807),#5528,.T.);
#5871=ADVANCED_FACE('',(#808),#5529,.T.);
#5872=ADVANCED_FACE('',(#809),#460,.T.);
#5873=ADVANCED_FACE('',(#810),#461,.T.);
#5874=ADVANCED_FACE('',(#811),#462,.T.);
#5875=ADVANCED_FACE('',(#812),#463,.T.);
#5876=ADVANCED_FACE('',(#813),#464,.T.);
#5877=ADVANCED_FACE('',(#814),#465,.T.);
#5878=ADVANCED_FACE('',(#815),#466,.T.);
#5879=CLOSED_SHELL('',(#5530,#5531,#5532,#5533,#5534,#5535,#5536,#5537,
#5538,#5539,#5540,#5541,#5542,#5543,#5544,#5545,#5546,#5547));
#5880=CLOSED_SHELL('',(#5548,#5549,#5550,#5551,#5552,#5553,#5554,#5555,
#5556,#5557,#5558,#5559,#5560,#5561,#5562,#5563,#5564,#5565,#5566,#5567,
#5568,#5569,#5570,#5571,#5572,#5573,#5574));
#5881=CLOSED_SHELL('',(#5575,#5576,#5577,#5578,#5579,#5580,#5581,#5582,
#5583,#5584,#5585,#5586,#5587,#5588,#5589,#5590,#5591,#5592,#5593,#5594,
#5595,#5596,#5597,#5598,#5599,#5600,#5601,#5602,#5603,#5604,#5605,#5606,
#5607,#5608,#5609,#5610,#5611,#5612,#5613,#5614,#5615,#5616,#5617,#5618,
#5619,#5620,#5621,#5622,#5623,#5624,#5625,#5626,#5627,#5628));
#5882=CLOSED_SHELL('',(#5629,#5630,#5631,#5632,#5633,#5634,#5635,#5636,
#5637,#5638,#5639,#5640,#5641,#5642,#5643,#5644,#5645,#5646,#5647,#5648,
#5649,#5650,#5651,#5652,#5653,#5654,#5655,#5656,#5657,#5658,#5659,#5660,
#5661,#5662,#5663,#5664,#5665,#5666));
#5883=CLOSED_SHELL('',(#5667,#5668,#5669,#5670,#5671,#5672,#5673,#5674,
#5675,#5676,#5677,#5678,#5679,#5680,#5681,#5682,#5683,#5684,#5685,#5686,
#5687,#5688,#5689,#5690,#5691,#5692,#5693,#5694,#5695,#5696,#5697,#5698,
#5699,#5700,#5701,#5702));
#5884=CLOSED_SHELL('',(#5703,#5704,#5705,#5706,#5707,#5708,#5709,#5710,
#5711,#5712,#5713,#5714));
#5885=CLOSED_SHELL('',(#5715,#5716,#5717,#5718,#5719,#5720,#5721,#5722,
#5723,#5724,#5725,#5726,#5727,#5728,#5729,#5730,#5731,#5732,#5733,#5734,
#5735,#5736,#5737,#5738,#5739,#5740,#5741,#5742,#5743,#5744,#5745,#5746,
#5747,#5748,#5749,#5750,#5751,#5752,#5753,#5754,#5755,#5756));
#5886=CLOSED_SHELL('',(#5757,#5758,#5759,#5760,#5761,#5762,#5763,#5764,
#5765,#5766,#5767,#5768,#5769,#5770,#5771,#5772,#5773,#5774,#5775,#5776,
#5777,#5778,#5779,#5780,#5781,#5782,#5783,#5784,#5785,#5786,#5787,#5788,
#5789,#5790,#5791,#5792,#5793,#5794,#5795,#5796,#5797,#5798));
#5887=CLOSED_SHELL('',(#5799,#5800,#5801,#5802,#5803,#5804,#5805,#5806,
#5807,#5808,#5809,#5810,#5811,#5812,#5813,#5814,#5815,#5816,#5817,#5818,
#5819,#5820,#5821,#5822,#5823,#5824,#5825,#5826,#5827,#5828,#5829,#5830,
#5831,#5832,#5833,#5834,#5835,#5836,#5837,#5838,#5839,#5840));
#5888=CLOSED_SHELL('',(#5841,#5842,#5843,#5844,#5845,#5846,#5847,#5848,
#5849,#5850,#5851,#5852,#5853,#5854,#5855,#5856,#5857,#5858,#5859,#5860,
#5861,#5862,#5863,#5864,#5865,#5866,#5867,#5868,#5869,#5870,#5871,#5872,
#5873,#5874,#5875,#5876,#5877,#5878));
#5889=DERIVED_UNIT_ELEMENT(#5909,1.);
#5890=DERIVED_UNIT_ELEMENT(#10133,-3.);
#5891=DERIVED_UNIT_ELEMENT(#5909,1.);
#5892=DERIVED_UNIT_ELEMENT(#10133,-3.);
#5893=DERIVED_UNIT_ELEMENT(#5909,1.);
#5894=DERIVED_UNIT_ELEMENT(#10133,-3.);
#5895=DERIVED_UNIT_ELEMENT(#5909,1.);
#5896=DERIVED_UNIT_ELEMENT(#10133,-3.);
#5897=DERIVED_UNIT_ELEMENT(#5909,1.);
#5898=DERIVED_UNIT_ELEMENT(#10133,-3.);
#5899=DERIVED_UNIT_ELEMENT(#5909,1.);
#5900=DERIVED_UNIT_ELEMENT(#10133,-3.);
#5901=DERIVED_UNIT_ELEMENT(#5909,1.);
#5902=DERIVED_UNIT_ELEMENT(#10133,-3.);
#5903=DERIVED_UNIT_ELEMENT(#5909,1.);
#5904=DERIVED_UNIT_ELEMENT(#10133,-3.);
#5905=DERIVED_UNIT_ELEMENT(#5909,1.);
#5906=DERIVED_UNIT_ELEMENT(#10133,-3.);
#5907=DERIVED_UNIT_ELEMENT(#5909,1.);
#5908=DERIVED_UNIT_ELEMENT(#10133,-3.);
#5909=(
MASS_UNIT()
NAMED_UNIT(*)
SI_UNIT(.KILO.,.GRAM.)
);
#5910=DERIVED_UNIT((#5889,#5890));
#5911=DERIVED_UNIT((#5891,#5892));
#5912=DERIVED_UNIT((#5893,#5894));
#5913=DERIVED_UNIT((#5895,#5896));
#5914=DERIVED_UNIT((#5897,#5898));
#5915=DERIVED_UNIT((#5899,#5900));
#5916=DERIVED_UNIT((#5901,#5902));
#5917=DERIVED_UNIT((#5903,#5904));
#5918=DERIVED_UNIT((#5905,#5906));
#5919=DERIVED_UNIT((#5907,#5908));
#5920=MEASURE_REPRESENTATION_ITEM('density measure',
POSITIVE_RATIO_MEASURE(7850.),#5910);
#5921=MEASURE_REPRESENTATION_ITEM('density measure',
POSITIVE_RATIO_MEASURE(7850.),#5911);
#5922=MEASURE_REPRESENTATION_ITEM('density measure',
POSITIVE_RATIO_MEASURE(7850.),#5912);
#5923=MEASURE_REPRESENTATION_ITEM('density measure',
POSITIVE_RATIO_MEASURE(7850.),#5913);
#5924=MEASURE_REPRESENTATION_ITEM('density measure',
POSITIVE_RATIO_MEASURE(7850.),#5914);
#5925=MEASURE_REPRESENTATION_ITEM('density measure',
POSITIVE_RATIO_MEASURE(7850.),#5915);
#5926=MEASURE_REPRESENTATION_ITEM('density measure',
POSITIVE_RATIO_MEASURE(7850.),#5916);
#5927=MEASURE_REPRESENTATION_ITEM('density measure',
POSITIVE_RATIO_MEASURE(7850.),#5917);
#5928=MEASURE_REPRESENTATION_ITEM('density measure',
POSITIVE_RATIO_MEASURE(7850.),#5918);
#5929=MEASURE_REPRESENTATION_ITEM('density measure',
POSITIVE_RATIO_MEASURE(7850.),#5919);
#5930=PROPERTY_DEFINITION_REPRESENTATION(#5980,#5950);
#5931=PROPERTY_DEFINITION_REPRESENTATION(#5981,#5951);
#5932=PROPERTY_DEFINITION_REPRESENTATION(#5982,#5952);
#5933=PROPERTY_DEFINITION_REPRESENTATION(#5983,#5953);
#5934=PROPERTY_DEFINITION_REPRESENTATION(#5984,#5954);
#5935=PROPERTY_DEFINITION_REPRESENTATION(#5985,#5955);
#5936=PROPERTY_DEFINITION_REPRESENTATION(#5986,#5956);
#5937=PROPERTY_DEFINITION_REPRESENTATION(#5987,#5957);
#5938=PROPERTY_DEFINITION_REPRESENTATION(#5988,#5958);
#5939=PROPERTY_DEFINITION_REPRESENTATION(#5989,#5959);
#5940=PROPERTY_DEFINITION_REPRESENTATION(#5990,#5960);
#5941=PROPERTY_DEFINITION_REPRESENTATION(#5991,#5961);
#5942=PROPERTY_DEFINITION_REPRESENTATION(#5992,#5962);
#5943=PROPERTY_DEFINITION_REPRESENTATION(#5993,#5963);
#5944=PROPERTY_DEFINITION_REPRESENTATION(#5994,#5964);
#5945=PROPERTY_DEFINITION_REPRESENTATION(#5995,#5965);
#5946=PROPERTY_DEFINITION_REPRESENTATION(#5996,#5966);
#5947=PROPERTY_DEFINITION_REPRESENTATION(#5997,#5967);
#5948=PROPERTY_DEFINITION_REPRESENTATION(#5998,#5968);
#5949=PROPERTY_DEFINITION_REPRESENTATION(#5999,#5969);
#5950=REPRESENTATION('material name',(#5970),#10121);
#5951=REPRESENTATION('density',(#5920),#10121);
#5952=REPRESENTATION('material name',(#5971),#10122);
#5953=REPRESENTATION('density',(#5921),#10122);
#5954=REPRESENTATION('material name',(#5972),#10123);
#5955=REPRESENTATION('density',(#5922),#10123);
#5956=REPRESENTATION('material name',(#5973),#10124);
#5957=REPRESENTATION('density',(#5923),#10124);
#5958=REPRESENTATION('material name',(#5974),#10125);
#5959=REPRESENTATION('density',(#5924),#10125);
#5960=REPRESENTATION('material name',(#5975),#10126);
#5961=REPRESENTATION('density',(#5925),#10126);
#5962=REPRESENTATION('material name',(#5976),#10127);
#5963=REPRESENTATION('density',(#5926),#10127);
#5964=REPRESENTATION('material name',(#5977),#10128);
#5965=REPRESENTATION('density',(#5927),#10128);
#5966=REPRESENTATION('material name',(#5978),#10129);
#5967=REPRESENTATION('density',(#5928),#10129);
#5968=REPRESENTATION('material name',(#5979),#10130);
#5969=REPRESENTATION('density',(#5929),#10130);
#5970=DESCRIPTIVE_REPRESENTATION_ITEM('Steel','Steel');
#5971=DESCRIPTIVE_REPRESENTATION_ITEM('Steel','Steel');
#5972=DESCRIPTIVE_REPRESENTATION_ITEM('Steel','Steel');
#5973=DESCRIPTIVE_REPRESENTATION_ITEM('Steel','Steel');
#5974=DESCRIPTIVE_REPRESENTATION_ITEM('Steel','Steel');
#5975=DESCRIPTIVE_REPRESENTATION_ITEM('Steel','Steel');
#5976=DESCRIPTIVE_REPRESENTATION_ITEM('Steel','Steel');
#5977=DESCRIPTIVE_REPRESENTATION_ITEM('Steel','Steel');
#5978=DESCRIPTIVE_REPRESENTATION_ITEM('Steel','Steel');
#5979=DESCRIPTIVE_REPRESENTATION_ITEM('Steel','Steel');
#5980=PROPERTY_DEFINITION('material property','material name',#10181);
#5981=PROPERTY_DEFINITION('material property','density of part',#10181);
#5982=PROPERTY_DEFINITION('material property','material name',#10182);
#5983=PROPERTY_DEFINITION('material property','density of part',#10182);
#5984=PROPERTY_DEFINITION('material property','material name',#10183);
#5985=PROPERTY_DEFINITION('material property','density of part',#10183);
#5986=PROPERTY_DEFINITION('material property','material name',#10184);
#5987=PROPERTY_DEFINITION('material property','density of part',#10184);
#5988=PROPERTY_DEFINITION('material property','material name',#10185);
#5989=PROPERTY_DEFINITION('material property','density of part',#10185);
#5990=PROPERTY_DEFINITION('material property','material name',#10186);
#5991=PROPERTY_DEFINITION('material property','density of part',#10186);
#5992=PROPERTY_DEFINITION('material property','material name',#10187);
#5993=PROPERTY_DEFINITION('material property','density of part',#10187);
#5994=PROPERTY_DEFINITION('material property','material name',#10188);
#5995=PROPERTY_DEFINITION('material property','density of part',#10188);
#5996=PROPERTY_DEFINITION('material property','material name',#10189);
#5997=PROPERTY_DEFINITION('material property','density of part',#10189);
#5998=PROPERTY_DEFINITION('material property','material name',#10190);
#5999=PROPERTY_DEFINITION('material property','density of part',#10190);
#6000=AXIS2_PLACEMENT_3D('',#8416,#6622,#6623);
#6001=AXIS2_PLACEMENT_3D('',#8417,#6624,#6625);
#6002=AXIS2_PLACEMENT_3D('',#8418,#6626,#6627);
#6003=AXIS2_PLACEMENT_3D('',#8420,#6628,#6629);
#6004=AXIS2_PLACEMENT_3D('',#8423,#6631,#6632);
#6005=AXIS2_PLACEMENT_3D('',#8424,#6633,#6634);
#6006=AXIS2_PLACEMENT_3D('',#8426,#6635,#6636);
#6007=AXIS2_PLACEMENT_3D('',#8429,#6638,#6639);
#6008=AXIS2_PLACEMENT_3D('',#8430,#6640,#6641);
#6009=AXIS2_PLACEMENT_3D('',#8432,#6642,#6643);
#6010=AXIS2_PLACEMENT_3D('',#8435,#6645,#6646);
#6011=AXIS2_PLACEMENT_3D('',#8436,#6647,#6648);
#6012=AXIS2_PLACEMENT_3D('',#8438,#6649,#6650);
#6013=AXIS2_PLACEMENT_3D('',#8441,#6652,#6653);
#6014=AXIS2_PLACEMENT_3D('',#8442,#6654,#6655);
#6015=AXIS2_PLACEMENT_3D('',#8444,#6656,#6657);
#6016=AXIS2_PLACEMENT_3D('',#8447,#6659,#6660);
#6017=AXIS2_PLACEMENT_3D('',#8448,#6661,#6662);
#6018=AXIS2_PLACEMENT_3D('',#8450,#6663,#6664);
#6019=AXIS2_PLACEMENT_3D('',#8453,#6666,#6667);
#6020=AXIS2_PLACEMENT_3D('',#8454,#6668,#6669);
#6021=AXIS2_PLACEMENT_3D('',#8456,#6670,#6671);
#6022=AXIS2_PLACEMENT_3D('',#8459,#6673,#6674);
#6023=AXIS2_PLACEMENT_3D('',#8460,#6675,#6676);
#6024=AXIS2_PLACEMENT_3D('',#8462,#6677,#6678);
#6025=AXIS2_PLACEMENT_3D('',#8465,#6680,#6681);
#6026=AXIS2_PLACEMENT_3D('',#8466,#6682,#6683);
#6027=AXIS2_PLACEMENT_3D('',#8469,#6684,#6685);
#6028=AXIS2_PLACEMENT_3D('',#8473,#6687,#6688);
#6029=AXIS2_PLACEMENT_3D('',#8475,#6690,#6691);
#6030=AXIS2_PLACEMENT_3D('',#8481,#6695,#6696);
#6031=AXIS2_PLACEMENT_3D('',#8485,#6698,#6699);
#6032=AXIS2_PLACEMENT_3D('',#8489,#6701,#6702);
#6033=AXIS2_PLACEMENT_3D('',#8492,#6704,#6705);
#6034=AXIS2_PLACEMENT_3D('',#8493,#6706,#6707);
#6035=AXIS2_PLACEMENT_3D('',#8496,#6708,#6709);
#6036=AXIS2_PLACEMENT_3D('',#8499,#6712,#6713);
#6037=AXIS2_PLACEMENT_3D('',#8503,#6716,#6717);
#6038=AXIS2_PLACEMENT_3D('',#8505,#6718,#6719);
#6039=AXIS2_PLACEMENT_3D('',#8507,#6721,#6722);
#6040=AXIS2_PLACEMENT_3D('',#8509,#6723,#6724);
#6041=AXIS2_PLACEMENT_3D('',#8511,#6726,#6727);
#6042=AXIS2_PLACEMENT_3D('',#8513,#6729,#6730);
#6043=AXIS2_PLACEMENT_3D('',#8515,#6732,#6733);
#6044=AXIS2_PLACEMENT_3D('',#8516,#6734,#6735);
#6045=AXIS2_PLACEMENT_3D('',#8517,#6736,#6737);
#6046=AXIS2_PLACEMENT_3D('',#8519,#6738,#6739);
#6047=AXIS2_PLACEMENT_3D('',#8522,#6741,#6742);
#6048=AXIS2_PLACEMENT_3D('',#8523,#6743,#6744);
#6049=AXIS2_PLACEMENT_3D('',#8532,#6749,#6750);
#6050=AXIS2_PLACEMENT_3D('',#8538,#6754,#6755);
#6051=AXIS2_PLACEMENT_3D('',#8544,#6759,#6760);
#6052=AXIS2_PLACEMENT_3D('',#8550,#6764,#6765);
#6053=AXIS2_PLACEMENT_3D('',#8556,#6769,#6770);
#6054=AXIS2_PLACEMENT_3D('',#8562,#6774,#6775);
#6055=AXIS2_PLACEMENT_3D('',#8568,#6779,#6780);
#6056=AXIS2_PLACEMENT_3D('',#8574,#6784,#6785);
#6057=AXIS2_PLACEMENT_3D('',#8580,#6789,#6790);
#6058=AXIS2_PLACEMENT_3D('',#8586,#6794,#6795);
#6059=AXIS2_PLACEMENT_3D('',#8592,#6799,#6800);
#6060=AXIS2_PLACEMENT_3D('',#8595,#6803,#6804);
#6061=AXIS2_PLACEMENT_3D('',#8601,#6808,#6809);
#6062=AXIS2_PLACEMENT_3D('',#8605,#6812,#6813);
#6063=AXIS2_PLACEMENT_3D('',#8609,#6816,#6817);
#6064=AXIS2_PLACEMENT_3D('',#8613,#6820,#6821);
#6065=AXIS2_PLACEMENT_3D('',#8617,#6824,#6825);
#6066=AXIS2_PLACEMENT_3D('',#8621,#6828,#6829);
#6067=AXIS2_PLACEMENT_3D('',#8622,#6830,#6831);
#6068=AXIS2_PLACEMENT_3D('',#8628,#6835,#6836);
#6069=AXIS2_PLACEMENT_3D('',#8632,#6839,#6840);
#6070=AXIS2_PLACEMENT_3D('',#8639,#6845,#6846);
#6071=AXIS2_PLACEMENT_3D('',#8641,#6848,#6849);
#6072=AXIS2_PLACEMENT_3D('',#8643,#6851,#6852);
#6073=AXIS2_PLACEMENT_3D('',#8644,#6853,#6854);
#6074=AXIS2_PLACEMENT_3D('',#8645,#6855,#6856);
#6075=AXIS2_PLACEMENT_3D('',#8646,#6857,#6858);
#6076=AXIS2_PLACEMENT_3D('',#8649,#6859,#6860);
#6077=AXIS2_PLACEMENT_3D('',#8651,#6861,#6862);
#6078=AXIS2_PLACEMENT_3D('',#8663,#6863,#6864);
#6079=AXIS2_PLACEMENT_3D('',#8664,#6865,#6866);
#6080=AXIS2_PLACEMENT_3D('',#8667,#6867,#6868);
#6081=AXIS2_PLACEMENT_3D('',#8670,#6871,#6872);
#6082=AXIS2_PLACEMENT_3D('',#8683,#6873,#6874);
#6083=AXIS2_PLACEMENT_3D('',#8684,#6875,#6876);
#6084=AXIS2_PLACEMENT_3D('',#8685,#6877,#6878);
#6085=AXIS2_PLACEMENT_3D('',#8691,#6882,#6883);
#6086=AXIS2_PLACEMENT_3D('',#8694,#6884,#6885);
#6087=AXIS2_PLACEMENT_3D('',#8696,#6886,#6887);
#6088=AXIS2_PLACEMENT_3D('',#8708,#6888,#6889);
#6089=AXIS2_PLACEMENT_3D('',#8709,#6890,#6891);
#6090=AXIS2_PLACEMENT_3D('',#8712,#6892,#6893);
#6091=AXIS2_PLACEMENT_3D('',#8715,#6896,#6897);
#6092=AXIS2_PLACEMENT_3D('',#8728,#6898,#6899);
#6093=AXIS2_PLACEMENT_3D('',#8729,#6900,#6901);
#6094=AXIS2_PLACEMENT_3D('',#8730,#6902,#6903);
#6095=AXIS2_PLACEMENT_3D('',#8736,#6907,#6908);
#6096=AXIS2_PLACEMENT_3D('',#8738,#6909,#6910);
#6097=AXIS2_PLACEMENT_3D('',#8741,#6912,#6913);
#6098=AXIS2_PLACEMENT_3D('',#8742,#6914,#6915);
#6099=AXIS2_PLACEMENT_3D('',#8744,#6916,#6917);
#6100=AXIS2_PLACEMENT_3D('',#8747,#6919,#6920);
#6101=AXIS2_PLACEMENT_3D('',#8748,#6921,#6922);
#6102=AXIS2_PLACEMENT_3D('',#8750,#6923,#6924);
#6103=AXIS2_PLACEMENT_3D('',#8753,#6926,#6927);
#6104=AXIS2_PLACEMENT_3D('',#8754,#6928,#6929);
#6105=AXIS2_PLACEMENT_3D('',#8756,#6930,#6931);
#6106=AXIS2_PLACEMENT_3D('',#8759,#6933,#6934);
#6107=AXIS2_PLACEMENT_3D('',#8760,#6935,#6936);
#6108=AXIS2_PLACEMENT_3D('',#8763,#6939,#6940);
#6109=AXIS2_PLACEMENT_3D('',#8767,#6942,#6943);
#6110=AXIS2_PLACEMENT_3D('',#8769,#6945,#6946);
#6111=AXIS2_PLACEMENT_3D('',#8773,#6948,#6949);
#6112=AXIS2_PLACEMENT_3D('',#8775,#6951,#6952);
#6113=AXIS2_PLACEMENT_3D('',#8783,#6957,#6958);
#6114=AXIS2_PLACEMENT_3D('',#8799,#6967,#6968);
#6115=AXIS2_PLACEMENT_3D('',#8801,#6969,#6970);
#6116=AXIS2_PLACEMENT_3D('',#8803,#6972,#6973);
#6117=AXIS2_PLACEMENT_3D('',#8806,#6975,#6976);
#6118=AXIS2_PLACEMENT_3D('',#8807,#6977,#6978);
#6119=AXIS2_PLACEMENT_3D('',#8812,#6980,#6981);
#6120=AXIS2_PLACEMENT_3D('',#8815,#6983,#6984);
#6121=AXIS2_PLACEMENT_3D('',#8816,#6985,#6986);
#6122=AXIS2_PLACEMENT_3D('',#8821,#6988,#6989);
#6123=AXIS2_PLACEMENT_3D('',#8824,#6991,#6992);
#6124=AXIS2_PLACEMENT_3D('',#8825,#6993,#6994);
#6125=AXIS2_PLACEMENT_3D('',#8829,#6996,#6997);
#6126=AXIS2_PLACEMENT_3D('',#8831,#6999,#7000);
#6127=AXIS2_PLACEMENT_3D('',#8836,#7002,#7003);
#6128=AXIS2_PLACEMENT_3D('',#8839,#7005,#7006);
#6129=AXIS2_PLACEMENT_3D('',#8840,#7007,#7008);
#6130=AXIS2_PLACEMENT_3D('',#8844,#7010,#7011);
#6131=AXIS2_PLACEMENT_3D('',#8846,#7013,#7014);
#6132=AXIS2_PLACEMENT_3D('',#8849,#7017,#7018);
#6133=AXIS2_PLACEMENT_3D('',#8854,#7021,#7022);
#6134=AXIS2_PLACEMENT_3D('',#8855,#7023,#7024);
#6135=AXIS2_PLACEMENT_3D('',#8860,#7027,#7028);
#6136=AXIS2_PLACEMENT_3D('',#8861,#7029,#7030);
#6137=AXIS2_PLACEMENT_3D('',#8864,#7033,#7034);
#6138=AXIS2_PLACEMENT_3D('',#8869,#7037,#7038);
#6139=AXIS2_PLACEMENT_3D('',#8870,#7039,#7040);
#6140=AXIS2_PLACEMENT_3D('',#8875,#7043,#7044);
#6141=AXIS2_PLACEMENT_3D('',#8876,#7045,#7046);
#6142=AXIS2_PLACEMENT_3D('',#8879,#7049,#7050);
#6143=AXIS2_PLACEMENT_3D('',#8884,#7054,#7055);
#6144=AXIS2_PLACEMENT_3D('',#8888,#7058,#7059);
#6145=AXIS2_PLACEMENT_3D('',#8892,#7062,#7063);
#6146=AXIS2_PLACEMENT_3D('',#8896,#7066,#7067);
#6147=AXIS2_PLACEMENT_3D('',#8900,#7070,#7071);
#6148=AXIS2_PLACEMENT_3D('',#8904,#7074,#7075);
#6149=AXIS2_PLACEMENT_3D('',#8905,#7076,#7077);
#6150=AXIS2_PLACEMENT_3D('',#8907,#7078,#7079);
#6151=AXIS2_PLACEMENT_3D('',#8909,#7081,#7082);
#6152=AXIS2_PLACEMENT_3D('',#8911,#7083,#7084);
#6153=AXIS2_PLACEMENT_3D('',#8913,#7086,#7087);
#6154=AXIS2_PLACEMENT_3D('',#8915,#7089,#7090);
#6155=AXIS2_PLACEMENT_3D('',#8916,#7091,#7092);
#6156=AXIS2_PLACEMENT_3D('',#8918,#7094,#7095);
#6157=AXIS2_PLACEMENT_3D('',#8919,#7096,#7097);
#6158=AXIS2_PLACEMENT_3D('',#8920,#7098,#7099);
#6159=AXIS2_PLACEMENT_3D('',#8921,#7100,#7101);
#6160=AXIS2_PLACEMENT_3D('',#8922,#7102,#7103);
#6161=AXIS2_PLACEMENT_3D('',#8923,#7104,#7105);
#6162=AXIS2_PLACEMENT_3D('',#8924,#7106,#7107);
#6163=AXIS2_PLACEMENT_3D('',#8925,#7108,#7109);
#6164=AXIS2_PLACEMENT_3D('',#8926,#7110,#7111);
#6165=AXIS2_PLACEMENT_3D('',#8927,#7112,#7113);
#6166=AXIS2_PLACEMENT_3D('',#8928,#7114,#7115);
#6167=AXIS2_PLACEMENT_3D('',#8929,#7116,#7117);
#6168=AXIS2_PLACEMENT_3D('',#8931,#7119,#7120);
#6169=AXIS2_PLACEMENT_3D('',#8933,#7122,#7123);
#6170=AXIS2_PLACEMENT_3D('',#8935,#7125,#7126);
#6171=AXIS2_PLACEMENT_3D('',#8937,#7128,#7129);
#6172=AXIS2_PLACEMENT_3D('',#8939,#7131,#7132);
#6173=AXIS2_PLACEMENT_3D('',#8940,#7133,#7134);
#6174=AXIS2_PLACEMENT_3D('',#8941,#7135,#7136);
#6175=AXIS2_PLACEMENT_3D('',#8946,#7138,#7139);
#6176=AXIS2_PLACEMENT_3D('',#8949,#7141,#7142);
#6177=AXIS2_PLACEMENT_3D('',#8950,#7143,#7144);
#6178=AXIS2_PLACEMENT_3D('',#8955,#7146,#7147);
#6179=AXIS2_PLACEMENT_3D('',#8958,#7149,#7150);
#6180=AXIS2_PLACEMENT_3D('',#8959,#7151,#7152);
#6181=AXIS2_PLACEMENT_3D('',#8963,#7154,#7155);
#6182=AXIS2_PLACEMENT_3D('',#8965,#7157,#7158);
#6183=AXIS2_PLACEMENT_3D('',#8969,#7160,#7161);
#6184=AXIS2_PLACEMENT_3D('',#8971,#7163,#7164);
#6185=AXIS2_PLACEMENT_3D('',#8975,#7166,#7167);
#6186=AXIS2_PLACEMENT_3D('',#8977,#7169,#7170);
#6187=AXIS2_PLACEMENT_3D('',#8981,#7172,#7173);
#6188=AXIS2_PLACEMENT_3D('',#8983,#7175,#7176);
#6189=AXIS2_PLACEMENT_3D('',#8988,#7179,#7180);
#6190=AXIS2_PLACEMENT_3D('',#8989,#7181,#7182);
#6191=AXIS2_PLACEMENT_3D('',#8994,#7185,#7186);
#6192=AXIS2_PLACEMENT_3D('',#8995,#7187,#7188);
#6193=AXIS2_PLACEMENT_3D('',#9000,#7191,#7192);
#6194=AXIS2_PLACEMENT_3D('',#9001,#7193,#7194);
#6195=AXIS2_PLACEMENT_3D('',#9006,#7197,#7198);
#6196=AXIS2_PLACEMENT_3D('',#9007,#7199,#7200);
#6197=AXIS2_PLACEMENT_3D('',#9010,#7203,#7204);
#6198=AXIS2_PLACEMENT_3D('',#9013,#7207,#7208);
#6199=AXIS2_PLACEMENT_3D('',#9019,#7212,#7213);
#6200=AXIS2_PLACEMENT_3D('',#9023,#7216,#7217);
#6201=AXIS2_PLACEMENT_3D('',#9027,#7220,#7221);
#6202=AXIS2_PLACEMENT_3D('',#9031,#7224,#7225);
#6203=AXIS2_PLACEMENT_3D('',#9035,#7228,#7229);
#6204=AXIS2_PLACEMENT_3D('',#9039,#7232,#7233);
#6205=AXIS2_PLACEMENT_3D('',#9040,#7234,#7235);
#6206=AXIS2_PLACEMENT_3D('',#9044,#7237,#7238);
#6207=AXIS2_PLACEMENT_3D('',#9045,#7239,#7240);
#6208=AXIS2_PLACEMENT_3D('',#9046,#7241,#7242);
#6209=AXIS2_PLACEMENT_3D('',#9049,#7244,#7245);
#6210=AXIS2_PLACEMENT_3D('',#9050,#7246,#7247);
#6211=AXIS2_PLACEMENT_3D('',#9053,#7249,#7250);
#6212=AXIS2_PLACEMENT_3D('',#9054,#7251,#7252);
#6213=AXIS2_PLACEMENT_3D('',#9057,#7254,#7255);
#6214=AXIS2_PLACEMENT_3D('',#9058,#7256,#7257);
#6215=AXIS2_PLACEMENT_3D('',#9062,#7259,#7260);
#6216=AXIS2_PLACEMENT_3D('',#9064,#7262,#7263);
#6217=AXIS2_PLACEMENT_3D('',#9069,#7266,#7267);
#6218=AXIS2_PLACEMENT_3D('',#9070,#7268,#7269);
#6219=AXIS2_PLACEMENT_3D('',#9075,#7272,#7273);
#6220=AXIS2_PLACEMENT_3D('',#9076,#7274,#7275);
#6221=AXIS2_PLACEMENT_3D('',#9081,#7278,#7279);
#6222=AXIS2_PLACEMENT_3D('',#9082,#7280,#7281);
#6223=AXIS2_PLACEMENT_3D('',#9087,#7284,#7285);
#6224=AXIS2_PLACEMENT_3D('',#9088,#7286,#7287);
#6225=AXIS2_PLACEMENT_3D('',#9092,#7290,#7291);
#6226=AXIS2_PLACEMENT_3D('',#9093,#7292,#7293);
#6227=AXIS2_PLACEMENT_3D('',#9096,#7295,#7296);
#6228=AXIS2_PLACEMENT_3D('',#9097,#7297,#7298);
#6229=AXIS2_PLACEMENT_3D('',#9099,#7300,#7301);
#6230=AXIS2_PLACEMENT_3D('',#9102,#7304,#7305);
#6231=AXIS2_PLACEMENT_3D('',#9104,#7307,#7308);
#6232=AXIS2_PLACEMENT_3D('',#9105,#7309,#7310);
#6233=AXIS2_PLACEMENT_3D('',#9106,#7311,#7312);
#6234=AXIS2_PLACEMENT_3D('',#9109,#7315,#7316);
#6235=AXIS2_PLACEMENT_3D('',#9110,#7317,#7318);
#6236=AXIS2_PLACEMENT_3D('',#9111,#7319,#7320);
#6237=AXIS2_PLACEMENT_3D('',#9112,#7321,#7322);
#6238=AXIS2_PLACEMENT_3D('',#9114,#7323,#7324);
#6239=AXIS2_PLACEMENT_3D('',#9117,#7326,#7327);
#6240=AXIS2_PLACEMENT_3D('',#9118,#7328,#7329);
#6241=AXIS2_PLACEMENT_3D('',#9120,#7330,#7331);
#6242=AXIS2_PLACEMENT_3D('',#9123,#7333,#7334);
#6243=AXIS2_PLACEMENT_3D('',#9124,#7335,#7336);
#6244=AXIS2_PLACEMENT_3D('',#9126,#7337,#7338);
#6245=AXIS2_PLACEMENT_3D('',#9129,#7340,#7341);
#6246=AXIS2_PLACEMENT_3D('',#9130,#7342,#7343);
#6247=AXIS2_PLACEMENT_3D('',#9132,#7344,#7345);
#6248=AXIS2_PLACEMENT_3D('',#9135,#7347,#7348);
#6249=AXIS2_PLACEMENT_3D('',#9136,#7349,#7350);
#6250=AXIS2_PLACEMENT_3D('',#9138,#7351,#7352);
#6251=AXIS2_PLACEMENT_3D('',#9141,#7354,#7355);
#6252=AXIS2_PLACEMENT_3D('',#9142,#7356,#7357);
#6253=AXIS2_PLACEMENT_3D('',#9144,#7358,#7359);
#6254=AXIS2_PLACEMENT_3D('',#9147,#7361,#7362);
#6255=AXIS2_PLACEMENT_3D('',#9148,#7363,#7364);
#6256=AXIS2_PLACEMENT_3D('',#9150,#7365,#7366);
#6257=AXIS2_PLACEMENT_3D('',#9153,#7368,#7369);
#6258=AXIS2_PLACEMENT_3D('',#9154,#7370,#7371);
#6259=AXIS2_PLACEMENT_3D('',#9156,#7372,#7373);
#6260=AXIS2_PLACEMENT_3D('',#9159,#7375,#7376);
#6261=AXIS2_PLACEMENT_3D('',#9160,#7377,#7378);
#6262=AXIS2_PLACEMENT_3D('',#9162,#7379,#7380);
#6263=AXIS2_PLACEMENT_3D('',#9165,#7382,#7383);
#6264=AXIS2_PLACEMENT_3D('',#9166,#7384,#7385);
#6265=AXIS2_PLACEMENT_3D('',#9168,#7386,#7387);
#6266=AXIS2_PLACEMENT_3D('',#9171,#7389,#7390);
#6267=AXIS2_PLACEMENT_3D('',#9172,#7391,#7392);
#6268=AXIS2_PLACEMENT_3D('',#9177,#7394,#7395);
#6269=AXIS2_PLACEMENT_3D('',#9180,#7397,#7398);
#6270=AXIS2_PLACEMENT_3D('',#9181,#7399,#7400);
#6271=AXIS2_PLACEMENT_3D('',#9185,#7402,#7403);
#6272=AXIS2_PLACEMENT_3D('',#9187,#7405,#7406);
#6273=AXIS2_PLACEMENT_3D('',#9191,#7408,#7409);
#6274=AXIS2_PLACEMENT_3D('',#9193,#7411,#7412);
#6275=AXIS2_PLACEMENT_3D('',#9197,#7414,#7415);
#6276=AXIS2_PLACEMENT_3D('',#9199,#7417,#7418);
#6277=AXIS2_PLACEMENT_3D('',#9204,#7421,#7422);
#6278=AXIS2_PLACEMENT_3D('',#9205,#7423,#7424);
#6279=AXIS2_PLACEMENT_3D('',#9210,#7427,#7428);
#6280=AXIS2_PLACEMENT_3D('',#9211,#7429,#7430);
#6281=AXIS2_PLACEMENT_3D('',#9216,#7433,#7434);
#6282=AXIS2_PLACEMENT_3D('',#9217,#7435,#7436);
#6283=AXIS2_PLACEMENT_3D('',#9220,#7439,#7440);
#6284=AXIS2_PLACEMENT_3D('',#9226,#7444,#7445);
#6285=AXIS2_PLACEMENT_3D('',#9230,#7448,#7449);
#6286=AXIS2_PLACEMENT_3D('',#9234,#7452,#7453);
#6287=AXIS2_PLACEMENT_3D('',#9238,#7456,#7457);
#6288=AXIS2_PLACEMENT_3D('',#9239,#7458,#7459);
#6289=AXIS2_PLACEMENT_3D('',#9243,#7461,#7462);
#6290=AXIS2_PLACEMENT_3D('',#9244,#7463,#7464);
#6291=AXIS2_PLACEMENT_3D('',#9245,#7465,#7466);
#6292=AXIS2_PLACEMENT_3D('',#9248,#7468,#7469);
#6293=AXIS2_PLACEMENT_3D('',#9249,#7470,#7471);
#6294=AXIS2_PLACEMENT_3D('',#9252,#7473,#7474);
#6295=AXIS2_PLACEMENT_3D('',#9253,#7475,#7476);
#6296=AXIS2_PLACEMENT_3D('',#9256,#7478,#7479);
#6297=AXIS2_PLACEMENT_3D('',#9257,#7480,#7481);
#6298=AXIS2_PLACEMENT_3D('',#9262,#7484,#7485);
#6299=AXIS2_PLACEMENT_3D('',#9263,#7486,#7487);
#6300=AXIS2_PLACEMENT_3D('',#9268,#7490,#7491);
#6301=AXIS2_PLACEMENT_3D('',#9269,#7492,#7493);
#6302=AXIS2_PLACEMENT_3D('',#9274,#7496,#7497);
#6303=AXIS2_PLACEMENT_3D('',#9275,#7498,#7499);
#6304=AXIS2_PLACEMENT_3D('',#9278,#7502,#7503);
#6305=AXIS2_PLACEMENT_3D('',#9281,#7506,#7507);
#6306=AXIS2_PLACEMENT_3D('',#9283,#7509,#7510);
#6307=AXIS2_PLACEMENT_3D('',#9284,#7511,#7512);
#6308=AXIS2_PLACEMENT_3D('',#9285,#7513,#7514);
#6309=AXIS2_PLACEMENT_3D('',#9286,#7515,#7516);
#6310=AXIS2_PLACEMENT_3D('',#9287,#7517,#7518);
#6311=AXIS2_PLACEMENT_3D('',#9289,#7519,#7520);
#6312=AXIS2_PLACEMENT_3D('',#9292,#7522,#7523);
#6313=AXIS2_PLACEMENT_3D('',#9293,#7524,#7525);
#6314=AXIS2_PLACEMENT_3D('',#9295,#7526,#7527);
#6315=AXIS2_PLACEMENT_3D('',#9298,#7529,#7530);
#6316=AXIS2_PLACEMENT_3D('',#9299,#7531,#7532);
#6317=AXIS2_PLACEMENT_3D('',#9316,#7541,#7542);
#6318=AXIS2_PLACEMENT_3D('',#9322,#7546,#7547);
#6319=AXIS2_PLACEMENT_3D('',#9326,#7550,#7551);
#6320=AXIS2_PLACEMENT_3D('',#9330,#7554,#7555);
#6321=AXIS2_PLACEMENT_3D('',#9334,#7558,#7559);
#6322=AXIS2_PLACEMENT_3D('',#9338,#7562,#7563);
#6323=AXIS2_PLACEMENT_3D('',#9342,#7566,#7567);
#6324=AXIS2_PLACEMENT_3D('',#9346,#7570,#7571);
#6325=AXIS2_PLACEMENT_3D('',#9348,#7573,#7574);
#6326=AXIS2_PLACEMENT_3D('',#9349,#7575,#7576);
#6327=AXIS2_PLACEMENT_3D('',#9350,#7577,#7578);
#6328=AXIS2_PLACEMENT_3D('',#9352,#7579,#7580);
#6329=AXIS2_PLACEMENT_3D('',#9355,#7582,#7583);
#6330=AXIS2_PLACEMENT_3D('',#9356,#7584,#7585);
#6331=AXIS2_PLACEMENT_3D('',#9357,#7586,#7587);
#6332=AXIS2_PLACEMENT_3D('',#9359,#7588,#7589);
#6333=AXIS2_PLACEMENT_3D('',#9362,#7591,#7592);
#6334=AXIS2_PLACEMENT_3D('',#9363,#7593,#7594);
#6335=AXIS2_PLACEMENT_3D('',#9364,#7595,#7596);
#6336=AXIS2_PLACEMENT_3D('',#9366,#7597,#7598);
#6337=AXIS2_PLACEMENT_3D('',#9369,#7600,#7601);
#6338=AXIS2_PLACEMENT_3D('',#9370,#7602,#7603);
#6339=AXIS2_PLACEMENT_3D('',#9371,#7604,#7605);
#6340=AXIS2_PLACEMENT_3D('',#9376,#7607,#7608);
#6341=AXIS2_PLACEMENT_3D('',#9379,#7610,#7611);
#6342=AXIS2_PLACEMENT_3D('',#9380,#7612,#7613);
#6343=AXIS2_PLACEMENT_3D('',#9385,#7616,#7617);
#6344=AXIS2_PLACEMENT_3D('',#9386,#7618,#7619);
#6345=AXIS2_PLACEMENT_3D('',#9391,#7622,#7623);
#6346=AXIS2_PLACEMENT_3D('',#9392,#7624,#7625);
#6347=AXIS2_PLACEMENT_3D('',#9395,#7628,#7629);
#6348=AXIS2_PLACEMENT_3D('',#9399,#7631,#7632);
#6349=AXIS2_PLACEMENT_3D('',#9403,#7634,#7635);
#6350=AXIS2_PLACEMENT_3D('',#9405,#7637,#7638);
#6351=AXIS2_PLACEMENT_3D('',#9425,#7649,#7650);
#6352=AXIS2_PLACEMENT_3D('',#9426,#7651,#7652);
#6353=AXIS2_PLACEMENT_3D('',#9430,#7654,#7655);
#6354=AXIS2_PLACEMENT_3D('',#9433,#7657,#7658);
#6355=AXIS2_PLACEMENT_3D('',#9434,#7659,#7660);
#6356=AXIS2_PLACEMENT_3D('',#9452,#7670,#7671);
#6357=AXIS2_PLACEMENT_3D('',#9455,#7673,#7674);
#6358=AXIS2_PLACEMENT_3D('',#9456,#7675,#7676);
#6359=AXIS2_PLACEMENT_3D('',#9458,#7677,#7678);
#6360=AXIS2_PLACEMENT_3D('',#9460,#7680,#7681);
#6361=AXIS2_PLACEMENT_3D('',#9464,#7684,#7685);
#6362=AXIS2_PLACEMENT_3D('',#9465,#7686,#7687);
#6363=AXIS2_PLACEMENT_3D('',#9466,#7688,#7689);
#6364=AXIS2_PLACEMENT_3D('',#9470,#7691,#7692);
#6365=AXIS2_PLACEMENT_3D('',#9471,#7693,#7694);
#6366=AXIS2_PLACEMENT_3D('',#9472,#7695,#7696);
#6367=AXIS2_PLACEMENT_3D('',#9475,#7698,#7699);
#6368=AXIS2_PLACEMENT_3D('',#9476,#7700,#7701);
#6369=AXIS2_PLACEMENT_3D('',#9479,#7703,#7704);
#6370=AXIS2_PLACEMENT_3D('',#9480,#7705,#7706);
#6371=AXIS2_PLACEMENT_3D('',#9483,#7708,#7709);
#6372=AXIS2_PLACEMENT_3D('',#9484,#7710,#7711);
#6373=AXIS2_PLACEMENT_3D('',#9487,#7713,#7714);
#6374=AXIS2_PLACEMENT_3D('',#9488,#7715,#7716);
#6375=AXIS2_PLACEMENT_3D('',#9490,#7718,#7719);
#6376=AXIS2_PLACEMENT_3D('',#9492,#7721,#7722);
#6377=AXIS2_PLACEMENT_3D('',#9498,#7726,#7727);
#6378=AXIS2_PLACEMENT_3D('',#9502,#7730,#7731);
#6379=AXIS2_PLACEMENT_3D('',#9506,#7734,#7735);
#6380=AXIS2_PLACEMENT_3D('',#9510,#7738,#7739);
#6381=AXIS2_PLACEMENT_3D('',#9511,#7740,#7741);
#6382=AXIS2_PLACEMENT_3D('',#9512,#7742,#7743);
#6383=AXIS2_PLACEMENT_3D('',#9513,#7744,#7745);
#6384=AXIS2_PLACEMENT_3D('',#9514,#7746,#7747);
#6385=AXIS2_PLACEMENT_3D('',#9515,#7748,#7749);
#6386=AXIS2_PLACEMENT_3D('',#9516,#7750,#7751);
#6387=AXIS2_PLACEMENT_3D('',#9517,#7752,#7753);
#6388=AXIS2_PLACEMENT_3D('',#9518,#7754,#7755);
#6389=AXIS2_PLACEMENT_3D('',#9519,#7756,#7757);
#6390=AXIS2_PLACEMENT_3D('',#9522,#7759,#7760);
#6391=AXIS2_PLACEMENT_3D('',#9523,#7761,#7762);
#6392=AXIS2_PLACEMENT_3D('',#9526,#7764,#7765);
#6393=AXIS2_PLACEMENT_3D('',#9527,#7766,#7767);
#6394=AXIS2_PLACEMENT_3D('',#9529,#7769,#7770);
#6395=AXIS2_PLACEMENT_3D('',#9531,#7772,#7773);
#6396=AXIS2_PLACEMENT_3D('',#9534,#7776,#7777);
#6397=AXIS2_PLACEMENT_3D('',#9535,#7778,#7779);
#6398=AXIS2_PLACEMENT_3D('',#9536,#7780,#7781);
#6399=AXIS2_PLACEMENT_3D('',#9537,#7782,#7783);
#6400=AXIS2_PLACEMENT_3D('',#9538,#7784,#7785);
#6401=AXIS2_PLACEMENT_3D('',#9540,#7786,#7787);
#6402=AXIS2_PLACEMENT_3D('',#9543,#7789,#7790);
#6403=AXIS2_PLACEMENT_3D('',#9544,#7791,#7792);
#6404=AXIS2_PLACEMENT_3D('',#9546,#7793,#7794);
#6405=AXIS2_PLACEMENT_3D('',#9549,#7796,#7797);
#6406=AXIS2_PLACEMENT_3D('',#9550,#7798,#7799);
#6407=AXIS2_PLACEMENT_3D('',#9552,#7800,#7801);
#6408=AXIS2_PLACEMENT_3D('',#9555,#7803,#7804);
#6409=AXIS2_PLACEMENT_3D('',#9556,#7805,#7806);
#6410=AXIS2_PLACEMENT_3D('',#9558,#7807,#7808);
#6411=AXIS2_PLACEMENT_3D('',#9561,#7810,#7811);
#6412=AXIS2_PLACEMENT_3D('',#9562,#7812,#7813);
#6413=AXIS2_PLACEMENT_3D('',#9567,#7815,#7816);
#6414=AXIS2_PLACEMENT_3D('',#9570,#7818,#7819);
#6415=AXIS2_PLACEMENT_3D('',#9571,#7820,#7821);
#6416=AXIS2_PLACEMENT_3D('',#9576,#7823,#7824);
#6417=AXIS2_PLACEMENT_3D('',#9579,#7826,#7827);
#6418=AXIS2_PLACEMENT_3D('',#9580,#7828,#7829);
#6419=AXIS2_PLACEMENT_3D('',#9584,#7831,#7832);
#6420=AXIS2_PLACEMENT_3D('',#9586,#7834,#7835);
#6421=AXIS2_PLACEMENT_3D('',#9591,#7837,#7838);
#6422=AXIS2_PLACEMENT_3D('',#9594,#7840,#7841);
#6423=AXIS2_PLACEMENT_3D('',#9595,#7842,#7843);
#6424=AXIS2_PLACEMENT_3D('',#9599,#7845,#7846);
#6425=AXIS2_PLACEMENT_3D('',#9601,#7848,#7849);
#6426=AXIS2_PLACEMENT_3D('',#9604,#7852,#7853);
#6427=AXIS2_PLACEMENT_3D('',#9609,#7856,#7857);
#6428=AXIS2_PLACEMENT_3D('',#9610,#7858,#7859);
#6429=AXIS2_PLACEMENT_3D('',#9615,#7862,#7863);
#6430=AXIS2_PLACEMENT_3D('',#9616,#7864,#7865);
#6431=AXIS2_PLACEMENT_3D('',#9619,#7868,#7869);
#6432=AXIS2_PLACEMENT_3D('',#9624,#7872,#7873);
#6433=AXIS2_PLACEMENT_3D('',#9625,#7874,#7875);
#6434=AXIS2_PLACEMENT_3D('',#9630,#7878,#7879);
#6435=AXIS2_PLACEMENT_3D('',#9631,#7880,#7881);
#6436=AXIS2_PLACEMENT_3D('',#9634,#7884,#7885);
#6437=AXIS2_PLACEMENT_3D('',#9640,#7889,#7890);
#6438=AXIS2_PLACEMENT_3D('',#9644,#7893,#7894);
#6439=AXIS2_PLACEMENT_3D('',#9648,#7897,#7898);
#6440=AXIS2_PLACEMENT_3D('',#9652,#7901,#7902);
#6441=AXIS2_PLACEMENT_3D('',#9656,#7905,#7906);
#6442=AXIS2_PLACEMENT_3D('',#9660,#7909,#7910);
#6443=AXIS2_PLACEMENT_3D('',#9661,#7911,#7912);
#6444=AXIS2_PLACEMENT_3D('',#9666,#7914,#7915);
#6445=AXIS2_PLACEMENT_3D('',#9669,#7917,#7918);
#6446=AXIS2_PLACEMENT_3D('',#9670,#7919,#7920);
#6447=AXIS2_PLACEMENT_3D('',#9674,#7922,#7923);
#6448=AXIS2_PLACEMENT_3D('',#9676,#7925,#7926);
#6449=AXIS2_PLACEMENT_3D('',#9680,#7928,#7929);
#6450=AXIS2_PLACEMENT_3D('',#9682,#7931,#7932);
#6451=AXIS2_PLACEMENT_3D('',#9686,#7934,#7935);
#6452=AXIS2_PLACEMENT_3D('',#9688,#7937,#7938);
#6453=AXIS2_PLACEMENT_3D('',#9691,#7940,#7941);
#6454=AXIS2_PLACEMENT_3D('',#9693,#7943,#7944);
#6455=AXIS2_PLACEMENT_3D('',#9696,#7946,#7947);
#6456=AXIS2_PLACEMENT_3D('',#9697,#7948,#7949);
#6457=AXIS2_PLACEMENT_3D('',#9700,#7951,#7952);
#6458=AXIS2_PLACEMENT_3D('',#9701,#7953,#7954);
#6459=AXIS2_PLACEMENT_3D('',#9704,#7956,#7957);
#6460=AXIS2_PLACEMENT_3D('',#9705,#7958,#7959);
#6461=AXIS2_PLACEMENT_3D('',#9708,#7961,#7962);
#6462=AXIS2_PLACEMENT_3D('',#9709,#7963,#7964);
#6463=AXIS2_PLACEMENT_3D('',#9712,#7966,#7967);
#6464=AXIS2_PLACEMENT_3D('',#9713,#7968,#7969);
#6465=AXIS2_PLACEMENT_3D('',#9716,#7971,#7972);
#6466=AXIS2_PLACEMENT_3D('',#9717,#7973,#7974);
#6467=AXIS2_PLACEMENT_3D('',#9720,#7977,#7978);
#6468=AXIS2_PLACEMENT_3D('',#9722,#7980,#7981);
#6469=AXIS2_PLACEMENT_3D('',#9724,#7983,#7984);
#6470=AXIS2_PLACEMENT_3D('',#9725,#7985,#7986);
#6471=AXIS2_PLACEMENT_3D('',#9727,#7988,#7989);
#6472=AXIS2_PLACEMENT_3D('',#9729,#7991,#7992);
#6473=AXIS2_PLACEMENT_3D('',#9731,#7994,#7995);
#6474=AXIS2_PLACEMENT_3D('',#9732,#7996,#7997);
#6475=AXIS2_PLACEMENT_3D('',#9733,#7998,#7999);
#6476=AXIS2_PLACEMENT_3D('',#9735,#8000,#8001);
#6477=AXIS2_PLACEMENT_3D('',#9738,#8003,#8004);
#6478=AXIS2_PLACEMENT_3D('',#9739,#8005,#8006);
#6479=AXIS2_PLACEMENT_3D('',#9741,#8007,#8008);
#6480=AXIS2_PLACEMENT_3D('',#9744,#8010,#8011);
#6481=AXIS2_PLACEMENT_3D('',#9745,#8012,#8013);
#6482=AXIS2_PLACEMENT_3D('',#9747,#8014,#8015);
#6483=AXIS2_PLACEMENT_3D('',#9750,#8017,#8018);
#6484=AXIS2_PLACEMENT_3D('',#9751,#8019,#8020);
#6485=AXIS2_PLACEMENT_3D('',#9753,#8021,#8022);
#6486=AXIS2_PLACEMENT_3D('',#9756,#8024,#8025);
#6487=AXIS2_PLACEMENT_3D('',#9757,#8026,#8027);
#6488=AXIS2_PLACEMENT_3D('',#9762,#8029,#8030);
#6489=AXIS2_PLACEMENT_3D('',#9765,#8032,#8033);
#6490=AXIS2_PLACEMENT_3D('',#9766,#8034,#8035);
#6491=AXIS2_PLACEMENT_3D('',#9771,#8037,#8038);
#6492=AXIS2_PLACEMENT_3D('',#9774,#8040,#8041);
#6493=AXIS2_PLACEMENT_3D('',#9775,#8042,#8043);
#6494=AXIS2_PLACEMENT_3D('',#9779,#8045,#8046);
#6495=AXIS2_PLACEMENT_3D('',#9781,#8048,#8049);
#6496=AXIS2_PLACEMENT_3D('',#9786,#8051,#8052);
#6497=AXIS2_PLACEMENT_3D('',#9789,#8054,#8055);
#6498=AXIS2_PLACEMENT_3D('',#9790,#8056,#8057);
#6499=AXIS2_PLACEMENT_3D('',#9794,#8059,#8060);
#6500=AXIS2_PLACEMENT_3D('',#9796,#8062,#8063);
#6501=AXIS2_PLACEMENT_3D('',#9799,#8066,#8067);
#6502=AXIS2_PLACEMENT_3D('',#9804,#8070,#8071);
#6503=AXIS2_PLACEMENT_3D('',#9805,#8072,#8073);
#6504=AXIS2_PLACEMENT_3D('',#9810,#8076,#8077);
#6505=AXIS2_PLACEMENT_3D('',#9811,#8078,#8079);
#6506=AXIS2_PLACEMENT_3D('',#9814,#8082,#8083);
#6507=AXIS2_PLACEMENT_3D('',#9819,#8086,#8087);
#6508=AXIS2_PLACEMENT_3D('',#9820,#8088,#8089);
#6509=AXIS2_PLACEMENT_3D('',#9825,#8092,#8093);
#6510=AXIS2_PLACEMENT_3D('',#9826,#8094,#8095);
#6511=AXIS2_PLACEMENT_3D('',#9829,#8098,#8099);
#6512=AXIS2_PLACEMENT_3D('',#9835,#8103,#8104);
#6513=AXIS2_PLACEMENT_3D('',#9839,#8107,#8108);
#6514=AXIS2_PLACEMENT_3D('',#9843,#8111,#8112);
#6515=AXIS2_PLACEMENT_3D('',#9847,#8115,#8116);
#6516=AXIS2_PLACEMENT_3D('',#9851,#8119,#8120);
#6517=AXIS2_PLACEMENT_3D('',#9855,#8123,#8124);
#6518=AXIS2_PLACEMENT_3D('',#9856,#8125,#8126);
#6519=AXIS2_PLACEMENT_3D('',#9861,#8128,#8129);
#6520=AXIS2_PLACEMENT_3D('',#9864,#8131,#8132);
#6521=AXIS2_PLACEMENT_3D('',#9865,#8133,#8134);
#6522=AXIS2_PLACEMENT_3D('',#9869,#8136,#8137);
#6523=AXIS2_PLACEMENT_3D('',#9871,#8139,#8140);
#6524=AXIS2_PLACEMENT_3D('',#9875,#8142,#8143);
#6525=AXIS2_PLACEMENT_3D('',#9877,#8145,#8146);
#6526=AXIS2_PLACEMENT_3D('',#9881,#8148,#8149);
#6527=AXIS2_PLACEMENT_3D('',#9883,#8151,#8152);
#6528=AXIS2_PLACEMENT_3D('',#9886,#8154,#8155);
#6529=AXIS2_PLACEMENT_3D('',#9888,#8157,#8158);
#6530=AXIS2_PLACEMENT_3D('',#9891,#8160,#8161);
#6531=AXIS2_PLACEMENT_3D('',#9892,#8162,#8163);
#6532=AXIS2_PLACEMENT_3D('',#9895,#8165,#8166);
#6533=AXIS2_PLACEMENT_3D('',#9896,#8167,#8168);
#6534=AXIS2_PLACEMENT_3D('',#9899,#8170,#8171);
#6535=AXIS2_PLACEMENT_3D('',#9900,#8172,#8173);
#6536=AXIS2_PLACEMENT_3D('',#9903,#8175,#8176);
#6537=AXIS2_PLACEMENT_3D('',#9904,#8177,#8178);
#6538=AXIS2_PLACEMENT_3D('',#9907,#8180,#8181);
#6539=AXIS2_PLACEMENT_3D('',#9908,#8182,#8183);
#6540=AXIS2_PLACEMENT_3D('',#9911,#8185,#8186);
#6541=AXIS2_PLACEMENT_3D('',#9912,#8187,#8188);
#6542=AXIS2_PLACEMENT_3D('',#9915,#8191,#8192);
#6543=AXIS2_PLACEMENT_3D('',#9917,#8194,#8195);
#6544=AXIS2_PLACEMENT_3D('',#9919,#8197,#8198);
#6545=AXIS2_PLACEMENT_3D('',#9920,#8199,#8200);
#6546=AXIS2_PLACEMENT_3D('',#9922,#8202,#8203);
#6547=AXIS2_PLACEMENT_3D('',#9924,#8205,#8206);
#6548=AXIS2_PLACEMENT_3D('',#9926,#8208,#8209);
#6549=AXIS2_PLACEMENT_3D('',#9927,#8210,#8211);
#6550=AXIS2_PLACEMENT_3D('',#9928,#8212,#8213);
#6551=AXIS2_PLACEMENT_3D('',#9933,#8215,#8216);
#6552=AXIS2_PLACEMENT_3D('',#9936,#8218,#8219);
#6553=AXIS2_PLACEMENT_3D('',#9937,#8220,#8221);
#6554=AXIS2_PLACEMENT_3D('',#9942,#8223,#8224);
#6555=AXIS2_PLACEMENT_3D('',#9945,#8226,#8227);
#6556=AXIS2_PLACEMENT_3D('',#9946,#8228,#8229);
#6557=AXIS2_PLACEMENT_3D('',#9950,#8231,#8232);
#6558=AXIS2_PLACEMENT_3D('',#9952,#8234,#8235);
#6559=AXIS2_PLACEMENT_3D('',#9956,#8237,#8238);
#6560=AXIS2_PLACEMENT_3D('',#9958,#8240,#8241);
#6561=AXIS2_PLACEMENT_3D('',#9962,#8243,#8244);
#6562=AXIS2_PLACEMENT_3D('',#9964,#8246,#8247);
#6563=AXIS2_PLACEMENT_3D('',#9968,#8249,#8250);
#6564=AXIS2_PLACEMENT_3D('',#9970,#8252,#8253);
#6565=AXIS2_PLACEMENT_3D('',#9975,#8256,#8257);
#6566=AXIS2_PLACEMENT_3D('',#9976,#8258,#8259);
#6567=AXIS2_PLACEMENT_3D('',#9981,#8262,#8263);
#6568=AXIS2_PLACEMENT_3D('',#9982,#8264,#8265);
#6569=AXIS2_PLACEMENT_3D('',#9987,#8268,#8269);
#6570=AXIS2_PLACEMENT_3D('',#9988,#8270,#8271);
#6571=AXIS2_PLACEMENT_3D('',#9993,#8274,#8275);
#6572=AXIS2_PLACEMENT_3D('',#9994,#8276,#8277);
#6573=AXIS2_PLACEMENT_3D('',#9997,#8280,#8281);
#6574=AXIS2_PLACEMENT_3D('',#10000,#8284,#8285);
#6575=AXIS2_PLACEMENT_3D('',#10006,#8289,#8290);
#6576=AXIS2_PLACEMENT_3D('',#10010,#8293,#8294);
#6577=AXIS2_PLACEMENT_3D('',#10014,#8297,#8298);
#6578=AXIS2_PLACEMENT_3D('',#10018,#8301,#8302);
#6579=AXIS2_PLACEMENT_3D('',#10022,#8305,#8306);
#6580=AXIS2_PLACEMENT_3D('',#10026,#8309,#8310);
#6581=AXIS2_PLACEMENT_3D('',#10027,#8311,#8312);
#6582=AXIS2_PLACEMENT_3D('',#10031,#8314,#8315);
#6583=AXIS2_PLACEMENT_3D('',#10032,#8316,#8317);
#6584=AXIS2_PLACEMENT_3D('',#10033,#8318,#8319);
#6585=AXIS2_PLACEMENT_3D('',#10036,#8321,#8322);
#6586=AXIS2_PLACEMENT_3D('',#10037,#8323,#8324);
#6587=AXIS2_PLACEMENT_3D('',#10040,#8326,#8327);
#6588=AXIS2_PLACEMENT_3D('',#10041,#8328,#8329);
#6589=AXIS2_PLACEMENT_3D('',#10044,#8331,#8332);
#6590=AXIS2_PLACEMENT_3D('',#10045,#8333,#8334);
#6591=AXIS2_PLACEMENT_3D('',#10049,#8336,#8337);
#6592=AXIS2_PLACEMENT_3D('',#10051,#8339,#8340);
#6593=AXIS2_PLACEMENT_3D('',#10056,#8343,#8344);
#6594=AXIS2_PLACEMENT_3D('',#10057,#8345,#8346);
#6595=AXIS2_PLACEMENT_3D('',#10062,#8349,#8350);
#6596=AXIS2_PLACEMENT_3D('',#10063,#8351,#8352);
#6597=AXIS2_PLACEMENT_3D('',#10068,#8355,#8356);
#6598=AXIS2_PLACEMENT_3D('',#10069,#8357,#8358);
#6599=AXIS2_PLACEMENT_3D('',#10074,#8361,#8362);
#6600=AXIS2_PLACEMENT_3D('',#10075,#8363,#8364);
#6601=AXIS2_PLACEMENT_3D('',#10079,#8367,#8368);
#6602=AXIS2_PLACEMENT_3D('',#10080,#8369,#8370);
#6603=AXIS2_PLACEMENT_3D('',#10083,#8372,#8373);
#6604=AXIS2_PLACEMENT_3D('',#10084,#8374,#8375);
#6605=AXIS2_PLACEMENT_3D('',#10086,#8377,#8378);
#6606=AXIS2_PLACEMENT_3D('',#10089,#8381,#8382);
#6607=AXIS2_PLACEMENT_3D('',#10091,#8384,#8385);
#6608=AXIS2_PLACEMENT_3D('',#10092,#8386,#8387);
#6609=AXIS2_PLACEMENT_3D('',#10093,#8388,#8389);
#6610=AXIS2_PLACEMENT_3D('',#10096,#8392,#8393);
#6611=AXIS2_PLACEMENT_3D('',#10097,#8394,#8395);
#6612=AXIS2_PLACEMENT_3D('',#10098,#8396,#8397);
#6613=AXIS2_PLACEMENT_3D('',#10099,#8398,#8399);
#6614=AXIS2_PLACEMENT_3D('',#10100,#8400,#8401);
#6615=AXIS2_PLACEMENT_3D('',#10101,#8402,#8403);
#6616=AXIS2_PLACEMENT_3D('',#10102,#8404,#8405);
#6617=AXIS2_PLACEMENT_3D('',#10103,#8406,#8407);
#6618=AXIS2_PLACEMENT_3D('',#10104,#8408,#8409);
#6619=AXIS2_PLACEMENT_3D('',#10105,#8410,#8411);
#6620=AXIS2_PLACEMENT_3D('',#10106,#8412,#8413);
#6621=AXIS2_PLACEMENT_3D('',#10107,#8414,#8415);
#6622=DIRECTION('axis',(0.,0.,1.));
#6623=DIRECTION('refdir',(1.,0.,0.));
#6624=DIRECTION('axis',(0.,0.,1.));
#6625=DIRECTION('refdir',(1.,0.,0.));
#6626=DIRECTION('center_axis',(0.,0.,-1.));
#6627=DIRECTION('ref_axis',(1.83697019872103E-16,1.,0.));
#6628=DIRECTION('center_axis',(0.,0.,-1.));
#6629=DIRECTION('ref_axis',(1.83697019872103E-16,1.,0.));
#6630=DIRECTION('',(0.,0.,-1.));
#6631=DIRECTION('center_axis',(0.,0.,1.));
#6632=DIRECTION('ref_axis',(1.83697019872103E-16,1.,0.));
#6633=DIRECTION('center_axis',(0.,0.,-1.));
#6634=DIRECTION('ref_axis',(1.83697019872103E-16,1.,0.));
#6635=DIRECTION('center_axis',(0.,0.,-1.));
#6636=DIRECTION('ref_axis',(1.83697019872103E-16,1.,0.));
#6637=DIRECTION('',(0.,0.,-1.));
#6638=DIRECTION('center_axis',(0.,0.,1.));
#6639=DIRECTION('ref_axis',(1.83697019872103E-16,1.,0.));
#6640=DIRECTION('center_axis',(0.,0.,-1.));
#6641=DIRECTION('ref_axis',(1.,-1.22464679914735E-16,0.));
#6642=DIRECTION('center_axis',(0.,0.,-1.));
#6643=DIRECTION('ref_axis',(1.,-1.22464679914735E-16,0.));
#6644=DIRECTION('',(0.,0.,-1.));
#6645=DIRECTION('center_axis',(0.,0.,1.));
#6646=DIRECTION('ref_axis',(1.,-1.22464679914735E-16,0.));
#6647=DIRECTION('center_axis',(0.,0.,-1.));
#6648=DIRECTION('ref_axis',(1.,-1.22464679914735E-16,0.));
#6649=DIRECTION('center_axis',(0.,0.,-1.));
#6650=DIRECTION('ref_axis',(1.,-1.22464679914735E-16,0.));
#6651=DIRECTION('',(0.,0.,-1.));
#6652=DIRECTION('center_axis',(0.,0.,1.));
#6653=DIRECTION('ref_axis',(1.,-1.22464679914735E-16,0.));
#6654=DIRECTION('center_axis',(0.,0.,-1.));
#6655=DIRECTION('ref_axis',(-6.12323399573677E-17,-1.,0.));
#6656=DIRECTION('center_axis',(0.,0.,-1.));
#6657=DIRECTION('ref_axis',(-6.12323399573677E-17,-1.,0.));
#6658=DIRECTION('',(0.,0.,-1.));
#6659=DIRECTION('center_axis',(0.,0.,1.));
#6660=DIRECTION('ref_axis',(-6.12323399573677E-17,-1.,0.));
#6661=DIRECTION('center_axis',(0.,0.,-1.));
#6662=DIRECTION('ref_axis',(-6.12323399573677E-17,-1.,0.));
#6663=DIRECTION('center_axis',(0.,0.,-1.));
#6664=DIRECTION('ref_axis',(-6.12323399573677E-17,-1.,0.));
#6665=DIRECTION('',(0.,0.,-1.));
#6666=DIRECTION('center_axis',(0.,0.,1.));
#6667=DIRECTION('ref_axis',(-6.12323399573677E-17,-1.,0.));
#6668=DIRECTION('center_axis',(0.,0.,-1.));
#6669=DIRECTION('ref_axis',(-1.,0.,0.));
#6670=DIRECTION('center_axis',(0.,0.,-1.));
#6671=DIRECTION('ref_axis',(-1.,0.,0.));
#6672=DIRECTION('',(0.,0.,-1.));
#6673=DIRECTION('center_axis',(0.,0.,1.));
#6674=DIRECTION('ref_axis',(-1.,0.,0.));
#6675=DIRECTION('center_axis',(0.,0.,-1.));
#6676=DIRECTION('ref_axis',(-1.,0.,0.));
#6677=DIRECTION('center_axis',(0.,0.,-1.));
#6678=DIRECTION('ref_axis',(-1.,0.,0.));
#6679=DIRECTION('',(0.,0.,-1.));
#6680=DIRECTION('center_axis',(0.,0.,1.));
#6681=DIRECTION('ref_axis',(-1.,0.,0.));
#6682=DIRECTION('center_axis',(0.,0.,1.));
#6683=DIRECTION('ref_axis',(-0.707106781186547,0.707106781186547,0.));
#6684=DIRECTION('center_axis',(0.,0.,-1.));
#6685=DIRECTION('ref_axis',(-0.707106781186547,0.707106781186547,0.));
#6686=DIRECTION('',(0.,0.,-1.));
#6687=DIRECTION('center_axis',(0.,0.,1.));
#6688=DIRECTION('ref_axis',(-0.707106781186547,0.707106781186547,0.));
#6689=DIRECTION('',(0.,0.,1.));
#6690=DIRECTION('center_axis',(-1.,0.,0.));
#6691=DIRECTION('ref_axis',(0.,-1.,0.));
#6692=DIRECTION('',(0.,1.,0.));
#6693=DIRECTION('',(0.,0.,-1.));
#6694=DIRECTION('',(0.,-1.,0.));
#6695=DIRECTION('center_axis',(0.,0.,1.));
#6696=DIRECTION('ref_axis',(1.,0.,0.));
#6697=DIRECTION('',(1.,0.,0.));
#6698=DIRECTION('center_axis',(0.,0.,1.));
#6699=DIRECTION('ref_axis',(0.707106781186547,0.707106781186547,0.));
#6700=DIRECTION('',(0.,-1.,0.));
#6701=DIRECTION('center_axis',(0.,0.,1.));
#6702=DIRECTION('ref_axis',(0.707106781186547,-0.707106781186547,0.));
#6703=DIRECTION('',(-1.,0.,0.));
#6704=DIRECTION('center_axis',(0.,0.,1.));
#6705=DIRECTION('ref_axis',(-0.707106781186547,-0.707106781186547,0.));
#6706=DIRECTION('center_axis',(0.,0.,1.));
#6707=DIRECTION('ref_axis',(0.707106781186547,0.707106781186547,0.));
#6708=DIRECTION('center_axis',(0.,0.,-1.));
#6709=DIRECTION('ref_axis',(0.707106781186547,0.707106781186547,0.));
#6710=DIRECTION('',(0.,0.,-1.));
#6711=DIRECTION('',(0.,0.,1.));
#6712=DIRECTION('center_axis',(1.,0.,0.));
#6713=DIRECTION('ref_axis',(0.,1.,0.));
#6714=DIRECTION('',(0.,1.,0.));
#6715=DIRECTION('',(0.,0.,1.));
#6716=DIRECTION('center_axis',(0.,0.,1.));
#6717=DIRECTION('ref_axis',(0.707106781186547,-0.707106781186547,0.));
#6718=DIRECTION('center_axis',(0.,0.,-1.));
#6719=DIRECTION('ref_axis',(0.707106781186547,-0.707106781186547,0.));
#6720=DIRECTION('',(0.,0.,-1.));
#6721=DIRECTION('center_axis',(0.,0.,1.));
#6722=DIRECTION('ref_axis',(-0.707106781186547,-0.707106781186547,0.));
#6723=DIRECTION('center_axis',(0.,0.,-1.));
#6724=DIRECTION('ref_axis',(-0.707106781186547,-0.707106781186547,0.));
#6725=DIRECTION('',(0.,0.,1.));
#6726=DIRECTION('center_axis',(0.,-1.,0.));
#6727=DIRECTION('ref_axis',(1.,0.,0.));
#6728=DIRECTION('',(1.,0.,0.));
#6729=DIRECTION('center_axis',(0.,1.,0.));
#6730=DIRECTION('ref_axis',(-1.,0.,0.));
#6731=DIRECTION('',(-1.,0.,0.));
#6732=DIRECTION('center_axis',(0.,0.,1.));
#6733=DIRECTION('ref_axis',(1.,0.,0.));
#6734=DIRECTION('axis',(0.,0.,1.));
#6735=DIRECTION('refdir',(1.,0.,0.));
#6736=DIRECTION('center_axis',(-1.,0.,0.));
#6737=DIRECTION('ref_axis',(0.,1.,0.));
#6738=DIRECTION('center_axis',(-1.,0.,0.));
#6739=DIRECTION('ref_axis',(0.,1.,0.));
#6740=DIRECTION('',(-1.,0.,0.));
#6741=DIRECTION('center_axis',(1.,0.,0.));
#6742=DIRECTION('ref_axis',(0.,1.,0.));
#6743=DIRECTION('center_axis',(0.707106781186548,0.,0.707106781186548));
#6744=DIRECTION('ref_axis',(0.707106781186548,0.,-0.707106781186548));
#6745=DIRECTION('',(0.,1.,0.));
#6746=DIRECTION('',(-0.678598344545846,0.281084637714824,0.678598344545846));
#6747=DIRECTION('',(0.,-1.,0.));
#6748=DIRECTION('',(-0.678598344545848,0.281084637714818,0.678598344545848));
#6749=DIRECTION('center_axis',(0.707106781186549,0.499999999999999,0.499999999999999));
#6750=DIRECTION('ref_axis',(0.577350269189624,0.,-0.816496580927727));
#6751=DIRECTION('',(0.,0.707106781186548,-0.707106781186548));
#6752=DIRECTION('',(-0.678598344545845,0.678598344545848,0.281084637714821));
#6753=DIRECTION('',(0.,-0.707106781186548,0.707106781186548));
#6754=DIRECTION('center_axis',(0.707106781186549,0.707106781186546,0.));
#6755=DIRECTION('ref_axis',(0.,0.,-1.));
#6756=DIRECTION('',(0.,0.,-1.));
#6757=DIRECTION('',(-0.678598344545846,0.67859834454585,-0.281084637714816));
#6758=DIRECTION('',(0.,0.,1.));
#6759=DIRECTION('center_axis',(0.707106781186548,0.5,-0.5));
#6760=DIRECTION('ref_axis',(-0.577350269189625,0.,-0.816496580927726));
#6761=DIRECTION('',(0.,-0.707106781186548,-0.707106781186548));
#6762=DIRECTION('',(-0.678598344545847,0.281084637714819,-0.678598344545847));
#6763=DIRECTION('',(0.,0.707106781186548,0.707106781186548));
#6764=DIRECTION('center_axis',(0.707106781186548,0.,-0.707106781186548));
#6765=DIRECTION('ref_axis',(-0.707106781186548,0.,-0.707106781186548));
#6766=DIRECTION('',(0.,-1.,0.));
#6767=DIRECTION('',(-0.678598344545847,-0.281084637714822,-0.678598344545847));
#6768=DIRECTION('',(0.,1.,0.));
#6769=DIRECTION('center_axis',(0.707106781186548,-0.499999999999999,-0.500000000000001));
#6770=DIRECTION('ref_axis',(-0.577350269189627,0.,-0.816496580927725));
#6771=DIRECTION('',(0.,0.707106781186549,-0.707106781186546));
#6772=DIRECTION('',(0.,-0.707106781186549,0.707106781186546));
#6773=DIRECTION('',(-0.678598344545845,-0.678598344545848,-0.281084637714821));
#6774=DIRECTION('center_axis',(0.707106781186549,-0.707106781186546,0.));
#6775=DIRECTION('ref_axis',(0.,0.,-1.));
#6776=DIRECTION('',(0.,0.,-1.));
#6777=DIRECTION('',(0.,0.,1.));
#6778=DIRECTION('',(-0.678598344545846,-0.678598344545848,0.281084637714821));
#6779=DIRECTION('center_axis',(0.707106781186548,-0.499999999999999,0.500000000000001));
#6780=DIRECTION('ref_axis',(0.577350269189627,0.,-0.816496580927725));
#6781=DIRECTION('',(0.,-0.707106781186549,-0.707106781186546));
#6782=DIRECTION('',(0.,0.707106781186549,0.707106781186546));
#6783=DIRECTION('',(-0.678598344545847,-0.281084637714822,0.678598344545847));
#6784=DIRECTION('center_axis',(0.707106781186548,0.,0.707106781186548));
#6785=DIRECTION('ref_axis',(0.707106781186548,0.,-0.707106781186548));
#6786=DIRECTION('',(0.,-1.,0.));
#6787=DIRECTION('',(0.,1.,0.));
#6788=DIRECTION('',(-0.678598344545848,0.281084637714818,0.678598344545848));
#6789=DIRECTION('center_axis',(0.707106781186547,0.499999999999999,0.500000000000001));
#6790=DIRECTION('ref_axis',(0.577350269189627,0.,-0.816496580927725));
#6791=DIRECTION('',(0.,-0.707106781186549,0.707106781186546));
#6792=DIRECTION('',(0.,0.707106781186549,-0.707106781186546));
#6793=DIRECTION('',(-0.678598344545847,0.678598344545849,0.281084637714816));
#6794=DIRECTION('center_axis',(0.707106781186549,0.707106781186546,0.));
#6795=DIRECTION('ref_axis',(0.,0.,-1.));
#6796=DIRECTION('',(0.,0.,1.));
#6797=DIRECTION('',(0.,0.,-1.));
#6798=DIRECTION('',(-0.678598344545847,0.678598344545849,0.281084637714816));
#6799=DIRECTION('center_axis',(0.707106781186547,0.5,0.500000000000001));
#6800=DIRECTION('ref_axis',(0.577350269189627,0.,-0.816496580927726));
#6801=DIRECTION('',(0.,-0.707106781186548,0.707106781186547));
#6802=DIRECTION('',(0.,0.707106781186548,-0.707106781186547));
#6803=DIRECTION('center_axis',(0.,-0.707106781186546,0.707106781186549));
#6804=DIRECTION('ref_axis',(1.,0.,0.));
#6805=DIRECTION('',(-1.,0.,0.));
#6806=DIRECTION('',(0.,-0.707106781186549,-0.707106781186546));
#6807=DIRECTION('',(1.,0.,0.));
#6808=DIRECTION('center_axis',(0.,0.,1.));
#6809=DIRECTION('ref_axis',(0.,-1.,0.));
#6810=DIRECTION('',(1.,0.,0.));
#6811=DIRECTION('',(0.,-1.,0.));
#6812=DIRECTION('center_axis',(0.,0.707106781186546,0.707106781186549));
#6813=DIRECTION('ref_axis',(1.,0.,0.));
#6814=DIRECTION('',(-1.,0.,0.));
#6815=DIRECTION('',(0.,-0.707106781186549,0.707106781186546));
#6816=DIRECTION('center_axis',(0.,1.,0.));
#6817=DIRECTION('ref_axis',(0.,0.,1.));
#6818=DIRECTION('',(1.,0.,0.));
#6819=DIRECTION('',(0.,0.,1.));
#6820=DIRECTION('center_axis',(0.,0.707106781186547,0.707106781186548));
#6821=DIRECTION('ref_axis',(1.,0.,0.));
#6822=DIRECTION('',(-1.,0.,0.));
#6823=DIRECTION('',(0.,-0.707106781186548,0.707106781186547));
#6824=DIRECTION('center_axis',(0.,0.,1.));
#6825=DIRECTION('ref_axis',(0.,-1.,0.));
#6826=DIRECTION('',(1.,0.,0.));
#6827=DIRECTION('',(0.,-1.,0.));
#6828=DIRECTION('center_axis',(1.,0.,0.));
#6829=DIRECTION('ref_axis',(0.,0.,-1.));
#6830=DIRECTION('center_axis',(0.,-0.707106781186546,-0.707106781186549));
#6831=DIRECTION('ref_axis',(-1.,0.,0.));
#6832=DIRECTION('',(-1.,0.,0.));
#6833=DIRECTION('',(0.,0.707106781186549,-0.707106781186546));
#6834=DIRECTION('',(1.,0.,0.));
#6835=DIRECTION('center_axis',(0.,0.,-1.));
#6836=DIRECTION('ref_axis',(0.,1.,0.));
#6837=DIRECTION('',(0.,1.,0.));
#6838=DIRECTION('',(-1.,0.,0.));
#6839=DIRECTION('center_axis',(1.,0.,0.));
#6840=DIRECTION('ref_axis',(0.,1.,0.));
#6841=DIRECTION('',(0.,0.,-1.));
#6842=DIRECTION('',(0.,-0.707106781186548,0.707106781186548));
#6843=DIRECTION('',(0.,0.,1.));
#6844=DIRECTION('',(0.,0.707106781186548,0.707106781186548));
#6845=DIRECTION('center_axis',(0.,0.707106781186548,-0.707106781186548));
#6846=DIRECTION('ref_axis',(-1.,0.,0.));
#6847=DIRECTION('',(1.,0.,0.));
#6848=DIRECTION('center_axis',(0.,1.,0.));
#6849=DIRECTION('ref_axis',(0.,0.,1.));
#6850=DIRECTION('',(-1.,0.,0.));
#6851=DIRECTION('center_axis',(0.,0.707106781186548,0.707106781186548));
#6852=DIRECTION('ref_axis',(1.,0.,0.));
#6853=DIRECTION('center_axis',(0.,-1.,0.));
#6854=DIRECTION('ref_axis',(0.,0.,-1.));
#6855=DIRECTION('axis',(0.,0.,1.));
#6856=DIRECTION('refdir',(1.,0.,0.));
#6857=DIRECTION('center_axis',(-1.,0.,0.));
#6858=DIRECTION('ref_axis',(0.,0.,1.));
#6859=DIRECTION('center_axis',(0.,1.,0.));
#6860=DIRECTION('ref_axis',(1.,0.,0.));
#6861=DIRECTION('center_axis',(1.,0.,0.));
#6862=DIRECTION('ref_axis',(0.,-0.707106781186552,0.707106781186543));
#6863=DIRECTION('center_axis',(-1.,0.,0.));
#6864=DIRECTION('ref_axis',(0.,-0.707106781186552,0.707106781186543));
#6865=DIRECTION('center_axis',(0.,1.,0.));
#6866=DIRECTION('ref_axis',(0.707106781186546,0.,-0.707106781186549));
#6867=DIRECTION('center_axis',(0.,1.,0.));
#6868=DIRECTION('ref_axis',(1.,0.,0.));
#6869=DIRECTION('',(0.,-1.,0.));
#6870=DIRECTION('',(0.,1.,0.));
#6871=DIRECTION('center_axis',(-1.,0.,0.));
#6872=DIRECTION('ref_axis',(0.,0.,1.));
#6873=DIRECTION('center_axis',(1.,0.,0.));
#6874=DIRECTION('ref_axis',(0.,0.707106781186548,0.707106781186548));
#6875=DIRECTION('center_axis',(-1.,0.,0.));
#6876=DIRECTION('ref_axis',(0.,0.707106781186547,0.707106781186547));
#6877=DIRECTION('center_axis',(-1.,0.,0.));
#6878=DIRECTION('ref_axis',(0.,0.,1.));
#6879=DIRECTION('',(0.,0.,1.));
#6880=DIRECTION('',(0.,0.965925826289068,-0.258819045102522));
#6881=DIRECTION('',(0.,0.,-1.));
#6882=DIRECTION('center_axis',(1.,0.,0.));
#6883=DIRECTION('ref_axis',(0.,0.,-1.));
#6884=DIRECTION('center_axis',(0.,-1.,0.));
#6885=DIRECTION('ref_axis',(-1.,0.,0.));
#6886=DIRECTION('center_axis',(-1.,0.,0.));
#6887=DIRECTION('ref_axis',(0.,0.707106781186548,0.707106781186548));
#6888=DIRECTION('center_axis',(1.,0.,0.));
#6889=DIRECTION('ref_axis',(0.,0.707106781186547,0.707106781186547));
#6890=DIRECTION('center_axis',(0.,-1.,0.));
#6891=DIRECTION('ref_axis',(-0.707106781186546,0.,-0.707106781186549));
#6892=DIRECTION('center_axis',(0.,-1.,0.));
#6893=DIRECTION('ref_axis',(-1.,0.,0.));
#6894=DIRECTION('',(0.,1.,0.));
#6895=DIRECTION('',(0.,-1.,0.));
#6896=DIRECTION('center_axis',(1.,0.,0.));
#6897=DIRECTION('ref_axis',(0.,0.,-1.));
#6898=DIRECTION('center_axis',(-1.,0.,0.));
#6899=DIRECTION('ref_axis',(0.,-0.707106781186552,0.707106781186543));
#6900=DIRECTION('center_axis',(1.,0.,0.));
#6901=DIRECTION('ref_axis',(0.,-0.707106781186552,0.707106781186543));
#6902=DIRECTION('center_axis',(1.,0.,0.));
#6903=DIRECTION('ref_axis',(0.,0.,-1.));
#6904=DIRECTION('',(0.,0.,1.));
#6905=DIRECTION('',(0.,-0.965925826289068,0.258819045102522));
#6906=DIRECTION('',(0.,0.,-1.));
#6907=DIRECTION('center_axis',(0.,0.,-1.));
#6908=DIRECTION('ref_axis',(-1.,0.,0.));
#6909=DIRECTION('center_axis',(0.,0.,-1.));
#6910=DIRECTION('ref_axis',(-1.,0.,0.));
#6911=DIRECTION('',(0.,0.,-1.));
#6912=DIRECTION('center_axis',(0.,0.,1.));
#6913=DIRECTION('ref_axis',(-1.,0.,0.));
#6914=DIRECTION('center_axis',(0.,0.,-1.));
#6915=DIRECTION('ref_axis',(-1.,0.,0.));
#6916=DIRECTION('center_axis',(0.,0.,-1.));
#6917=DIRECTION('ref_axis',(-1.,0.,0.));
#6918=DIRECTION('',(0.,0.,-1.));
#6919=DIRECTION('center_axis',(0.,0.,1.));
#6920=DIRECTION('ref_axis',(-1.,0.,0.));
#6921=DIRECTION('center_axis',(0.,0.,-1.));
#6922=DIRECTION('ref_axis',(-1.,0.,0.));
#6923=DIRECTION('center_axis',(0.,0.,-1.));
#6924=DIRECTION('ref_axis',(-1.,0.,0.));
#6925=DIRECTION('',(0.,0.,-1.));
#6926=DIRECTION('center_axis',(0.,0.,1.));
#6927=DIRECTION('ref_axis',(-1.,0.,0.));
#6928=DIRECTION('center_axis',(0.,0.,-1.));
#6929=DIRECTION('ref_axis',(-1.,0.,0.));
#6930=DIRECTION('center_axis',(0.,0.,-1.));
#6931=DIRECTION('ref_axis',(-1.,0.,0.));
#6932=DIRECTION('',(0.,0.,-1.));
#6933=DIRECTION('center_axis',(0.,0.,1.));
#6934=DIRECTION('ref_axis',(-1.,0.,0.));
#6935=DIRECTION('center_axis',(0.,0.258819045102522,0.965925826289068));
#6936=DIRECTION('ref_axis',(0.,-0.965925826289068,0.258819045102522));
#6937=DIRECTION('',(1.,0.,0.));
#6938=DIRECTION('',(1.,0.,0.));
#6939=DIRECTION('center_axis',(-1.,0.,0.));
#6940=DIRECTION('ref_axis',(0.,0.707106781186554,0.707106781186541));
#6941=DIRECTION('',(-1.,0.,0.));
#6942=DIRECTION('center_axis',(-0.923879532511286,-0.382683432365092,0.));
#6943=DIRECTION('ref_axis',(-0.382683432365092,0.923879532511286,0.));
#6944=DIRECTION('',(1.,0.,0.));
#6945=DIRECTION('center_axis',(-1.,0.,0.));
#6946=DIRECTION('ref_axis',(0.,0.707106781186554,0.707106781186541));
#6947=DIRECTION('',(1.,0.,0.));
#6948=DIRECTION('center_axis',(-0.923879532511286,0.382683432365092,0.));
#6949=DIRECTION('ref_axis',(0.382683432365092,0.923879532511286,0.));
#6950=DIRECTION('',(-1.,0.,0.));
#6951=DIRECTION('center_axis',(0.,0.,1.));
#6952=DIRECTION('ref_axis',(1.,0.,0.));
#6953=DIRECTION('',(0.707106781186548,0.707106781186548,0.));
#6954=DIRECTION('',(0.,1.,0.));
#6955=DIRECTION('',(-0.707106781186548,0.707106781186548,0.));
#6956=DIRECTION('',(-1.,0.,0.));
#6957=DIRECTION('center_axis',(0.,0.,1.));
#6958=DIRECTION('ref_axis',(1.,0.,0.));
#6959=DIRECTION('',(-1.,0.,0.));
#6960=DIRECTION('',(-0.707106781186548,-0.707106781186548,0.));
#6961=DIRECTION('',(0.,-1.,0.));
#6962=DIRECTION('',(-0.707106781186548,-0.707106781186548,0.));
#6963=DIRECTION('',(-1.,-4.56509835347174E-16,0.));
#6964=DIRECTION('',(-0.707106781186548,-0.707106781186547,0.));
#6965=DIRECTION('',(0.,-1.,0.));
#6966=DIRECTION('',(0.707106781186548,-0.707106781186548,0.));
#6967=DIRECTION('center_axis',(1.,0.,0.));
#6968=DIRECTION('ref_axis',(0.,-0.707106781186554,0.707106781186541));
#6969=DIRECTION('center_axis',(0.923879532511286,-0.382683432365092,0.));
#6970=DIRECTION('ref_axis',(-0.382683432365092,-0.923879532511286,0.));
#6971=DIRECTION('',(1.,0.,0.));
#6972=DIRECTION('center_axis',(1.,0.,0.));
#6973=DIRECTION('ref_axis',(0.,-0.707106781186554,0.707106781186541));
#6974=DIRECTION('',(1.,0.,0.));
#6975=DIRECTION('center_axis',(0.923879532511283,0.382683432365099,0.));
#6976=DIRECTION('ref_axis',(-0.382683432365099,0.923879532511283,0.));
#6977=DIRECTION('center_axis',(-1.,0.,0.));
#6978=DIRECTION('ref_axis',(0.,-0.707106781186548,-0.707106781186548));
#6979=DIRECTION('',(1.,0.,0.));
#6980=DIRECTION('center_axis',(-0.923879532511283,-0.382683432365099,4.10284931589583E-15));
#6981=DIRECTION('ref_axis',(0.382683432365098,-0.923879532511283,9.90515446280861E-15));
#6982=DIRECTION('',(-1.,0.,0.));
#6983=DIRECTION('center_axis',(-0.923879532511286,0.382683432365092,0.));
#6984=DIRECTION('ref_axis',(0.382683432365091,0.923879532511286,0.));
#6985=DIRECTION('center_axis',(0.,1.,0.));
#6986=DIRECTION('ref_axis',(0.707106781186551,0.,-0.707106781186544));
#6987=DIRECTION('',(0.,1.,0.));
#6988=DIRECTION('center_axis',(-0.382683432365083,-0.92387953251129,0.));
#6989=DIRECTION('ref_axis',(0.923879532511289,-0.382683432365083,0.));
#6990=DIRECTION('',(0.,-1.,0.));
#6991=DIRECTION('center_axis',(0.382683432365097,0.923879532511284,8.49727915508632E-16));
#6992=DIRECTION('ref_axis',(0.923879532511284,-0.382683432365097,2.05142465794791E-15));
#6993=DIRECTION('center_axis',(0.707106781186548,0.707106781186548,0.));
#6994=DIRECTION('ref_axis',(0.499999999999996,-0.500000000000002,-0.707106781186549));
#6995=DIRECTION('',(0.707106781186548,0.707106781186548,0.));
#6996=DIRECTION('center_axis',(-0.92387953251129,-0.382683432365082,0.));
#6997=DIRECTION('ref_axis',(0.382683432365082,-0.92387953251129,0.));
#6998=DIRECTION('',(-0.707106781186548,-0.707106781186548,0.));
#6999=DIRECTION('center_axis',(0.,1.,0.));
#7000=DIRECTION('ref_axis',(0.707106781186548,0.,-0.707106781186548));
#7001=DIRECTION('',(0.,-1.,0.));
#7002=DIRECTION('center_axis',(0.382683432365093,0.923879532511285,0.));
#7003=DIRECTION('ref_axis',(0.923879532511285,-0.382683432365093,0.));
#7004=DIRECTION('',(0.,1.,0.));
#7005=DIRECTION('center_axis',(0.382683432365092,-0.923879532511286,0.));
#7006=DIRECTION('ref_axis',(-0.923879532511286,-0.382683432365092,0.));
#7007=DIRECTION('center_axis',(1.,4.56509835347174E-16,0.));
#7008=DIRECTION('ref_axis',(0.,-0.707106781186551,-0.707106781186544));
#7009=DIRECTION('',(1.,4.56509835347174E-16,0.));
#7010=DIRECTION('center_axis',(-0.923879532511287,-0.38268343236509,0.));
#7011=DIRECTION('ref_axis',(-0.38268343236509,0.923879532511287,0.));
#7012=DIRECTION('',(-1.,-4.56509835347174E-16,0.));
#7013=DIRECTION('center_axis',(0.707106781186548,0.707106781186547,0.));
#7014=DIRECTION('ref_axis',(0.5,-0.5,-0.707106781186547));
#7015=DIRECTION('',(-0.707106781186548,-0.707106781186547,0.));
#7016=DIRECTION('',(0.707106781186548,0.707106781186547,0.));
#7017=DIRECTION('center_axis',(-0.707106781186548,0.707106781186548,0.));
#7018=DIRECTION('ref_axis',(0.5,0.5,-0.707106781186547));
#7019=DIRECTION('',(0.707106781186548,-0.707106781186548,0.));
#7020=DIRECTION('',(-0.707106781186548,0.707106781186548,0.));
#7021=DIRECTION('center_axis',(0.923879532511286,-0.382683432365092,0.));
#7022=DIRECTION('ref_axis',(-0.382683432365091,-0.923879532511286,0.));
#7023=DIRECTION('center_axis',(-1.,0.,0.));
#7024=DIRECTION('ref_axis',(0.,0.707106781186548,-0.707106781186548));
#7025=DIRECTION('',(1.,0.,0.));
#7026=DIRECTION('',(-1.,0.,0.));
#7027=DIRECTION('center_axis',(0.923879532511286,0.382683432365092,0.));
#7028=DIRECTION('ref_axis',(0.382683432365092,-0.923879532511286,0.));
#7029=DIRECTION('center_axis',(0.707106781186548,0.707106781186548,0.));
#7030=DIRECTION('ref_axis',(0.5,-0.5,-0.707106781186547));
#7031=DIRECTION('',(0.707106781186548,0.707106781186548,0.));
#7032=DIRECTION('',(-0.707106781186548,-0.707106781186548,0.));
#7033=DIRECTION('center_axis',(-0.707106781186548,-0.707106781186548,0.));
#7034=DIRECTION('ref_axis',(-0.5,0.5,-0.707106781186547));
#7035=DIRECTION('',(0.707106781186548,0.707106781186548,0.));
#7036=DIRECTION('',(-0.707106781186548,-0.707106781186548,0.));
#7037=DIRECTION('center_axis',(0.382683432365092,0.923879532511286,0.));
#7038=DIRECTION('ref_axis',(0.923879532511286,-0.382683432365091,0.));
#7039=DIRECTION('center_axis',(0.,-1.,0.));
#7040=DIRECTION('ref_axis',(-0.707106781186548,0.,-0.707106781186548));
#7041=DIRECTION('',(0.,1.,0.));
#7042=DIRECTION('',(0.,-1.,0.));
#7043=DIRECTION('center_axis',(-0.382683432365092,0.923879532511286,0.));
#7044=DIRECTION('ref_axis',(0.923879532511286,0.382683432365092,0.));
#7045=DIRECTION('center_axis',(0.707106781186548,-0.707106781186548,0.));
#7046=DIRECTION('ref_axis',(-0.5,-0.5,-0.707106781186547));
#7047=DIRECTION('',(-0.707106781186548,0.707106781186548,0.));
#7048=DIRECTION('',(0.707106781186548,-0.707106781186548,0.));
#7049=DIRECTION('center_axis',(0.707106781186548,-0.707106781186548,0.));
#7050=DIRECTION('ref_axis',(0.,0.,-1.));
#7051=DIRECTION('',(0.,0.,1.));
#7052=DIRECTION('',(0.707106781186548,0.707106781186548,0.));
#7053=DIRECTION('',(0.,0.,-1.));
#7054=DIRECTION('center_axis',(1.,0.,0.));
#7055=DIRECTION('ref_axis',(0.,1.,0.));
#7056=DIRECTION('',(0.,0.,1.));
#7057=DIRECTION('',(0.,1.,0.));
#7058=DIRECTION('center_axis',(0.707106781186548,-0.707106781186548,0.));
#7059=DIRECTION('ref_axis',(0.707106781186548,0.707106781186548,0.));
#7060=DIRECTION('',(0.,0.,1.));
#7061=DIRECTION('',(0.707106781186548,0.707106781186548,0.));
#7062=DIRECTION('center_axis',(4.56509835347174E-16,-1.,0.));
#7063=DIRECTION('ref_axis',(1.,4.56509835347174E-16,0.));
#7064=DIRECTION('',(0.,0.,-1.));
#7065=DIRECTION('',(1.,4.56509835347174E-16,0.));
#7066=DIRECTION('center_axis',(0.707106781186547,-0.707106781186548,0.));
#7067=DIRECTION('ref_axis',(0.,0.,-1.));
#7068=DIRECTION('',(0.,0.,1.));
#7069=DIRECTION('',(0.707106781186548,0.707106781186547,0.));
#7070=DIRECTION('center_axis',(1.,0.,0.));
#7071=DIRECTION('ref_axis',(0.,1.,0.));
#7072=DIRECTION('',(0.,0.,1.));
#7073=DIRECTION('',(0.,1.,0.));
#7074=DIRECTION('center_axis',(0.,0.,1.));
#7075=DIRECTION('ref_axis',(1.,0.,0.));
#7076=DIRECTION('center_axis',(0.707106781186548,-0.707106781186548,0.));
#7077=DIRECTION('ref_axis',(-0.500000000000005,-0.500000000000005,0.707106781186541));
#7078=DIRECTION('center_axis',(0.382683432365092,-0.923879532511286,0.));
#7079=DIRECTION('ref_axis',(-0.923879532511286,-0.382683432365092,0.));
#7080=DIRECTION('',(0.707106781186548,-0.707106781186548,0.));
#7081=DIRECTION('center_axis',(0.,-1.,0.));
#7082=DIRECTION('ref_axis',(-0.707106781186554,0.,0.707106781186541));
#7083=DIRECTION('center_axis',(-0.382683432365092,-0.923879532511286,0.));
#7084=DIRECTION('ref_axis',(-0.923879532511286,0.382683432365092,0.));
#7085=DIRECTION('',(0.,-1.,0.));
#7086=DIRECTION('center_axis',(-0.707106781186548,-0.707106781186548,0.));
#7087=DIRECTION('ref_axis',(-0.500000000000005,0.500000000000005,0.707106781186541));
#7088=DIRECTION('',(-0.707106781186548,-0.707106781186548,0.));
#7089=DIRECTION('center_axis',(-0.707106781186548,0.707106781186548,0.));
#7090=DIRECTION('ref_axis',(0.500000000000005,0.500000000000005,0.707106781186541));
#7091=DIRECTION('center_axis',(-0.382683432365092,0.923879532511286,0.));
#7092=DIRECTION('ref_axis',(0.923879532511286,0.382683432365092,0.));
#7093=DIRECTION('',(-0.707106781186548,0.707106781186548,0.));
#7094=DIRECTION('center_axis',(0.,1.,0.));
#7095=DIRECTION('ref_axis',(0.707106781186554,0.,0.707106781186541));
#7096=DIRECTION('center_axis',(0.382683432365093,0.923879532511285,0.));
#7097=DIRECTION('ref_axis',(0.923879532511285,-0.382683432365093,0.));
#7098=DIRECTION('center_axis',(-0.707106781186548,-0.707106781186547,0.));
#7099=DIRECTION('ref_axis',(0.5,-0.5,0.707106781186547));
#7100=DIRECTION('center_axis',(0.923879532511287,0.38268343236509,0.));
#7101=DIRECTION('ref_axis',(-0.38268343236509,0.923879532511287,0.));
#7102=DIRECTION('center_axis',(1.,4.56509835347174E-16,0.));
#7103=DIRECTION('ref_axis',(0.,-0.707106781186557,0.707106781186538));
#7104=DIRECTION('center_axis',(0.92387953251129,0.382683432365082,0.));
#7105=DIRECTION('ref_axis',(-0.382683432365082,0.92387953251129,0.));
#7106=DIRECTION('center_axis',(0.707106781186548,0.707106781186548,0.));
#7107=DIRECTION('ref_axis',(0.500000000000005,-0.500000000000005,0.707106781186541));
#7108=DIRECTION('center_axis',(0.382683432365087,0.923879532511288,0.));
#7109=DIRECTION('ref_axis',(-0.923879532511288,0.382683432365087,0.));
#7110=DIRECTION('center_axis',(0.,1.,0.));
#7111=DIRECTION('ref_axis',(0.707106781186557,0.,0.707106781186538));
#7112=DIRECTION('center_axis',(0.382683432365097,0.923879532511284,-8.4972791550864E-16));
#7113=DIRECTION('ref_axis',(0.923879532511284,-0.382683432365097,-2.05142465794793E-15));
#7114=DIRECTION('center_axis',(-0.707106781186548,-0.707106781186548,0.));
#7115=DIRECTION('ref_axis',(0.5,-0.5,0.707106781186547));
#7116=DIRECTION('center_axis',(0.,-1.,0.));
#7117=DIRECTION('ref_axis',(1.,0.,0.));
#7118=DIRECTION('',(0.,0.,1.));
#7119=DIRECTION('center_axis',(-0.707106781186548,-0.707106781186548,0.));
#7120=DIRECTION('ref_axis',(0.707106781186548,-0.707106781186548,0.));
#7121=DIRECTION('',(0.,0.,1.));
#7122=DIRECTION('center_axis',(-1.,0.,0.));
#7123=DIRECTION('ref_axis',(0.,-1.,0.));
#7124=DIRECTION('',(0.,0.,1.));
#7125=DIRECTION('center_axis',(-0.707106781186548,0.707106781186548,0.));
#7126=DIRECTION('ref_axis',(-0.707106781186548,-0.707106781186548,0.));
#7127=DIRECTION('',(0.,0.,1.));
#7128=DIRECTION('center_axis',(0.,1.,0.));
#7129=DIRECTION('ref_axis',(-1.,0.,0.));
#7130=DIRECTION('',(0.,0.,1.));
#7131=DIRECTION('center_axis',(0.707106781186548,0.707106781186548,0.));
#7132=DIRECTION('ref_axis',(-0.707106781186548,0.707106781186548,0.));
#7133=DIRECTION('axis',(0.,0.,1.));
#7134=DIRECTION('refdir',(1.,0.,0.));
#7135=DIRECTION('center_axis',(0.,1.,0.));
#7136=DIRECTION('ref_axis',(0.707106781186548,0.,-0.707106781186548));
#7137=DIRECTION('',(0.,-1.,0.));
#7138=DIRECTION('center_axis',(0.38268343236509,0.923879532511287,0.));
#7139=DIRECTION('ref_axis',(0.923879532511287,-0.38268343236509,0.));
#7140=DIRECTION('',(0.,1.,0.));
#7141=DIRECTION('center_axis',(-0.382683432365087,-0.923879532511288,0.));
#7142=DIRECTION('ref_axis',(0.923879532511288,-0.382683432365087,0.));
#7143=DIRECTION('center_axis',(1.,0.,0.));
#7144=DIRECTION('ref_axis',(0.,-0.707106781186548,-0.707106781186548));
#7145=DIRECTION('',(1.,0.,0.));
#7146=DIRECTION('center_axis',(-0.923879532511287,-0.38268343236509,0.));
#7147=DIRECTION('ref_axis',(-0.38268343236509,0.923879532511287,0.));
#7148=DIRECTION('',(-1.,0.,0.));
#7149=DIRECTION('center_axis',(0.923879532511288,0.382683432365087,-5.80230514691304E-15));
#7150=DIRECTION('ref_axis',(-0.382683432365087,0.923879532511288,-1.40080037787048E-14));
#7151=DIRECTION('center_axis',(0.707106781186548,0.707106781186548,0.));
#7152=DIRECTION('ref_axis',(0.499999999999998,-0.499999999999998,-0.70710678118655));
#7153=DIRECTION('',(0.707106781186548,0.707106781186548,0.));
#7154=DIRECTION('center_axis',(-0.382683432365095,-0.923879532511285,0.));
#7155=DIRECTION('ref_axis',(-0.923879532511285,0.382683432365095,0.));
#7156=DIRECTION('',(-0.707106781186548,-0.707106781186548,0.));
#7157=DIRECTION('center_axis',(0.,-1.,0.));
#7158=DIRECTION('ref_axis',(0.707106781186548,0.,-0.707106781186548));
#7159=DIRECTION('',(0.,1.,0.));
#7160=DIRECTION('center_axis',(0.382683432365099,-0.923879532511283,-8.20569863179165E-15));
#7161=DIRECTION('ref_axis',(0.923879532511283,0.382683432365098,-1.98103089256172E-14));
#7162=DIRECTION('',(0.,-1.,0.));
#7163=DIRECTION('center_axis',(-0.707106781186548,0.707106781186548,0.));
#7164=DIRECTION('ref_axis',(0.499999999999998,0.499999999999998,-0.70710678118655));
#7165=DIRECTION('',(-0.707106781186548,0.707106781186548,0.));
#7166=DIRECTION('center_axis',(0.923879532511286,-0.382683432365092,0.));
#7167=DIRECTION('ref_axis',(-0.382683432365092,-0.923879532511286,0.));
#7168=DIRECTION('',(0.707106781186548,-0.707106781186548,0.));
#7169=DIRECTION('center_axis',(1.,0.,0.));
#7170=DIRECTION('ref_axis',(0.,0.707106781186548,-0.707106781186548));
#7171=DIRECTION('',(-1.,0.,0.));
#7172=DIRECTION('center_axis',(0.923879532511286,0.382683432365092,0.));
#7173=DIRECTION('ref_axis',(-0.382683432365092,0.923879532511286,0.));
#7174=DIRECTION('',(1.,0.,0.));
#7175=DIRECTION('center_axis',(-0.707106781186548,-0.707106781186548,0.));
#7176=DIRECTION('ref_axis',(-0.499999999999998,0.499999999999998,-0.70710678118655));
#7177=DIRECTION('',(0.707106781186548,0.707106781186548,0.));
#7178=DIRECTION('',(-0.707106781186548,-0.707106781186548,0.));
#7179=DIRECTION('center_axis',(0.382683432365092,0.923879532511286,0.));
#7180=DIRECTION('ref_axis',(0.923879532511286,-0.382683432365092,0.));
#7181=DIRECTION('center_axis',(0.,1.,0.));
#7182=DIRECTION('ref_axis',(-0.707106781186548,0.,-0.707106781186548));
#7183=DIRECTION('',(0.,1.,0.));
#7184=DIRECTION('',(0.,-1.,0.));
#7185=DIRECTION('center_axis',(-0.382683432365092,0.923879532511286,0.));
#7186=DIRECTION('ref_axis',(-0.923879532511286,-0.382683432365092,0.));
#7187=DIRECTION('center_axis',(0.707106781186548,-0.707106781186548,0.));
#7188=DIRECTION('ref_axis',(-0.499999999999998,-0.499999999999998,-0.70710678118655));
#7189=DIRECTION('',(-0.707106781186548,0.707106781186548,0.));
#7190=DIRECTION('',(0.707106781186548,-0.707106781186548,0.));
#7191=DIRECTION('center_axis',(-0.923879532511286,0.382683432365092,0.));
#7192=DIRECTION('ref_axis',(0.382683432365092,0.923879532511286,0.));
#7193=DIRECTION('center_axis',(-1.,0.,0.));
#7194=DIRECTION('ref_axis',(0.,-0.707106781186548,-0.707106781186548));
#7195=DIRECTION('',(-1.,0.,0.));
#7196=DIRECTION('',(1.,0.,0.));
#7197=DIRECTION('center_axis',(-0.923879532511286,-0.382683432365092,4.10284931589584E-15));
#7198=DIRECTION('ref_axis',(0.382683432365092,-0.923879532511286,9.90515446280885E-15));
#7199=DIRECTION('center_axis',(0.707106781186548,0.707106781186548,0.));
#7200=DIRECTION('ref_axis',(0.499999999999998,-0.499999999999998,-0.70710678118655));
#7201=DIRECTION('',(-0.707106781186548,-0.707106781186548,0.));
#7202=DIRECTION('',(0.707106781186548,0.707106781186548,0.));
#7203=DIRECTION('center_axis',(0.707106781186548,0.707106781186548,0.));
#7204=DIRECTION('ref_axis',(0.499999999999998,-0.499999999999998,-0.70710678118655));
#7205=DIRECTION('',(-0.707106781186548,-0.707106781186548,0.));
#7206=DIRECTION('',(0.707106781186548,0.707106781186548,0.));
#7207=DIRECTION('center_axis',(-0.707106781186548,-0.707106781186548,0.));
#7208=DIRECTION('ref_axis',(0.,0.,1.));
#7209=DIRECTION('',(0.,0.,1.));
#7210=DIRECTION('',(0.707106781186548,-0.707106781186548,0.));
#7211=DIRECTION('',(0.,0.,-1.));
#7212=DIRECTION('center_axis',(0.,-1.,0.));
#7213=DIRECTION('ref_axis',(1.,0.,0.));
#7214=DIRECTION('',(0.,0.,-1.));
#7215=DIRECTION('',(1.,0.,0.));
#7216=DIRECTION('center_axis',(0.707106781186548,-0.707106781186548,0.));
#7217=DIRECTION('ref_axis',(0.,0.,-1.));
#7218=DIRECTION('',(0.,0.,1.));
#7219=DIRECTION('',(0.707106781186548,0.707106781186548,0.));
#7220=DIRECTION('center_axis',(1.,0.,0.));
#7221=DIRECTION('ref_axis',(0.,1.,0.));
#7222=DIRECTION('',(0.,0.,-1.));
#7223=DIRECTION('',(0.,1.,0.));
#7224=DIRECTION('center_axis',(0.707106781186548,-0.707106781186548,0.));
#7225=DIRECTION('ref_axis',(0.,0.,-1.));
#7226=DIRECTION('',(0.,0.,1.));
#7227=DIRECTION('',(0.707106781186548,0.707106781186548,0.));
#7228=DIRECTION('center_axis',(0.,-1.,0.));
#7229=DIRECTION('ref_axis',(1.,0.,0.));
#7230=DIRECTION('',(0.,0.,-1.));
#7231=DIRECTION('',(1.,0.,0.));
#7232=DIRECTION('center_axis',(0.,0.,1.));
#7233=DIRECTION('ref_axis',(-1.,0.,0.));
#7234=DIRECTION('center_axis',(0.,1.,0.));
#7235=DIRECTION('ref_axis',(0.707106781186551,0.,0.707106781186544));
#7236=DIRECTION('',(0.,-1.,0.));
#7237=DIRECTION('center_axis',(0.38268343236509,0.923879532511287,0.));
#7238=DIRECTION('ref_axis',(0.923879532511287,-0.38268343236509,0.));
#7239=DIRECTION('center_axis',(0.382683432365087,0.923879532511288,0.));
#7240=DIRECTION('ref_axis',(0.923879532511288,-0.382683432365087,0.));
#7241=DIRECTION('center_axis',(-0.707106781186548,-0.707106781186548,0.));
#7242=DIRECTION('ref_axis',(0.499999999999998,-0.499999999999998,0.70710678118655));
#7243=DIRECTION('',(-0.707106781186548,-0.707106781186548,0.));
#7244=DIRECTION('center_axis',(0.923879532511285,0.382683432365095,-4.10284931589581E-15));
#7245=DIRECTION('ref_axis',(-0.382683432365095,0.923879532511285,9.905154462809E-15));
#7246=DIRECTION('center_axis',(1.,0.,0.));
#7247=DIRECTION('ref_axis',(0.,-0.707106781186548,0.707106781186548));
#7248=DIRECTION('',(-1.,0.,0.));
#7249=DIRECTION('center_axis',(0.923879532511286,-0.382683432365092,0.));
#7250=DIRECTION('ref_axis',(-0.382683432365092,-0.923879532511286,0.));
#7251=DIRECTION('center_axis',(-0.707106781186548,0.707106781186548,0.));
#7252=DIRECTION('ref_axis',(-0.499999999999998,-0.499999999999998,0.70710678118655));
#7253=DIRECTION('',(-0.707106781186548,0.707106781186548,0.));
#7254=DIRECTION('center_axis',(0.382683432365092,-0.923879532511286,0.));
#7255=DIRECTION('ref_axis',(0.923879532511286,0.382683432365092,0.));
#7256=DIRECTION('center_axis',(0.,-1.,0.));
#7257=DIRECTION('ref_axis',(-0.707106781186548,0.,0.707106781186548));
#7258=DIRECTION('',(0.,1.,0.));
#7259=DIRECTION('center_axis',(-0.382683432365092,-0.923879532511286,0.));
#7260=DIRECTION('ref_axis',(-0.923879532511286,0.382683432365092,0.));
#7261=DIRECTION('',(0.,-1.,0.));
#7262=DIRECTION('center_axis',(0.707106781186548,0.707106781186548,0.));
#7263=DIRECTION('ref_axis',(-0.499999999999998,0.499999999999998,0.70710678118655));
#7264=DIRECTION('',(-0.707106781186548,-0.707106781186548,0.));
#7265=DIRECTION('',(0.707106781186548,0.707106781186548,0.));
#7266=DIRECTION('center_axis',(-0.923879532511286,-0.382683432365092,0.));
#7267=DIRECTION('ref_axis',(0.382683432365092,-0.923879532511286,0.));
#7268=DIRECTION('center_axis',(-1.,0.,0.));
#7269=DIRECTION('ref_axis',(0.,0.707106781186548,0.707106781186548));
#7270=DIRECTION('',(-1.,0.,0.));
#7271=DIRECTION('',(1.,0.,0.));
#7272=DIRECTION('center_axis',(-0.923879532511286,0.382683432365092,0.));
#7273=DIRECTION('ref_axis',(0.382683432365092,0.923879532511286,0.));
#7274=DIRECTION('center_axis',(0.707106781186548,-0.707106781186548,0.));
#7275=DIRECTION('ref_axis',(0.499999999999998,0.499999999999998,0.70710678118655));
#7276=DIRECTION('',(-0.707106781186548,0.707106781186548,0.));
#7277=DIRECTION('',(0.707106781186548,-0.707106781186548,0.));
#7278=DIRECTION('center_axis',(-0.382683432365092,0.923879532511286,0.));
#7279=DIRECTION('ref_axis',(-0.923879532511286,-0.382683432365092,0.));
#7280=DIRECTION('center_axis',(0.,1.,0.));
#7281=DIRECTION('ref_axis',(0.707106781186548,0.,0.707106781186548));
#7282=DIRECTION('',(0.,1.,0.));
#7283=DIRECTION('',(0.,-1.,0.));
#7284=DIRECTION('center_axis',(0.382683432365092,0.923879532511286,-4.10284931589584E-15));
#7285=DIRECTION('ref_axis',(0.923879532511286,-0.382683432365092,-9.90515446280885E-15));
#7286=DIRECTION('center_axis',(-0.707106781186548,-0.707106781186548,0.));
#7287=DIRECTION('ref_axis',(0.499999999999998,-0.499999999999998,0.70710678118655));
#7288=DIRECTION('',(0.707106781186548,0.707106781186548,0.));
#7289=DIRECTION('',(-0.707106781186548,-0.707106781186548,0.));
#7290=DIRECTION('center_axis',(0.923879532511287,0.38268343236509,0.));
#7291=DIRECTION('ref_axis',(-0.38268343236509,0.923879532511287,0.));
#7292=DIRECTION('center_axis',(1.,0.,0.));
#7293=DIRECTION('ref_axis',(0.,-0.707106781186551,0.707106781186544));
#7294=DIRECTION('',(-1.,0.,0.));
#7295=DIRECTION('center_axis',(0.923879532511288,0.382683432365087,5.80230514691306E-15));
#7296=DIRECTION('ref_axis',(-0.382683432365087,0.923879532511288,1.40080037787049E-14));
#7297=DIRECTION('center_axis',(-0.707106781186548,-0.707106781186548,0.));
#7298=DIRECTION('ref_axis',(0.499999999999998,-0.499999999999998,0.70710678118655));
#7299=DIRECTION('',(-0.707106781186548,-0.707106781186548,0.));
#7300=DIRECTION('center_axis',(0.707106781186548,0.707106781186548,0.));
#7301=DIRECTION('ref_axis',(0.,0.,-1.));
#7302=DIRECTION('',(0.,0.,1.));
#7303=DIRECTION('',(0.,0.,-1.));
#7304=DIRECTION('center_axis',(1.,0.,0.));
#7305=DIRECTION('ref_axis',(0.,1.,0.));
#7306=DIRECTION('',(0.,0.,1.));
#7307=DIRECTION('center_axis',(0.707106781186548,-0.707106781186548,0.));
#7308=DIRECTION('ref_axis',(0.,0.,-1.));
#7309=DIRECTION('center_axis',(0.,0.,1.));
#7310=DIRECTION('ref_axis',(1.,0.,0.));
#7311=DIRECTION('center_axis',(-0.707106781186548,0.707106781186548,0.));
#7312=DIRECTION('ref_axis',(0.,0.,1.));
#7313=DIRECTION('',(0.,0.,1.));
#7314=DIRECTION('',(0.,0.,-1.));
#7315=DIRECTION('center_axis',(0.,1.,0.));
#7316=DIRECTION('ref_axis',(-1.,0.,0.));
#7317=DIRECTION('center_axis',(-1.,0.,0.));
#7318=DIRECTION('ref_axis',(0.,-1.,0.));
#7319=DIRECTION('axis',(0.,0.,1.));
#7320=DIRECTION('refdir',(1.,0.,0.));
#7321=DIRECTION('center_axis',(0.,1.,0.));
#7322=DIRECTION('ref_axis',(1.,0.,0.));
#7323=DIRECTION('center_axis',(0.,1.,0.));
#7324=DIRECTION('ref_axis',(1.,0.,0.));
#7325=DIRECTION('',(0.,1.,0.));
#7326=DIRECTION('center_axis',(0.,-1.,0.));
#7327=DIRECTION('ref_axis',(1.,0.,0.));
#7328=DIRECTION('center_axis',(0.,1.,0.));
#7329=DIRECTION('ref_axis',(1.,0.,0.));
#7330=DIRECTION('center_axis',(0.,1.,0.));
#7331=DIRECTION('ref_axis',(1.,0.,0.));
#7332=DIRECTION('',(0.,1.,0.));
#7333=DIRECTION('center_axis',(0.,-1.,0.));
#7334=DIRECTION('ref_axis',(1.,0.,0.));
#7335=DIRECTION('center_axis',(0.,1.,0.));
#7336=DIRECTION('ref_axis',(1.,0.,0.));
#7337=DIRECTION('center_axis',(0.,1.,0.));
#7338=DIRECTION('ref_axis',(1.,0.,0.));
#7339=DIRECTION('',(0.,1.,0.));
#7340=DIRECTION('center_axis',(0.,-1.,0.));
#7341=DIRECTION('ref_axis',(1.,0.,0.));
#7342=DIRECTION('center_axis',(0.,1.,0.));
#7343=DIRECTION('ref_axis',(1.,0.,0.));
#7344=DIRECTION('center_axis',(0.,1.,0.));
#7345=DIRECTION('ref_axis',(1.,0.,0.));
#7346=DIRECTION('',(0.,1.,0.));
#7347=DIRECTION('center_axis',(0.,-1.,0.));
#7348=DIRECTION('ref_axis',(1.,0.,0.));
#7349=DIRECTION('center_axis',(0.,1.,0.));
#7350=DIRECTION('ref_axis',(1.,0.,0.));
#7351=DIRECTION('center_axis',(0.,1.,0.));
#7352=DIRECTION('ref_axis',(1.,0.,0.));
#7353=DIRECTION('',(0.,1.,0.));
#7354=DIRECTION('center_axis',(0.,-1.,0.));
#7355=DIRECTION('ref_axis',(1.,0.,0.));
#7356=DIRECTION('center_axis',(0.,1.,0.));
#7357=DIRECTION('ref_axis',(1.,0.,0.));
#7358=DIRECTION('center_axis',(0.,1.,0.));
#7359=DIRECTION('ref_axis',(1.,0.,0.));
#7360=DIRECTION('',(0.,1.,0.));
#7361=DIRECTION('center_axis',(0.,-1.,0.));
#7362=DIRECTION('ref_axis',(1.,0.,0.));
#7363=DIRECTION('center_axis',(0.,1.,0.));
#7364=DIRECTION('ref_axis',(1.,0.,0.));
#7365=DIRECTION('center_axis',(0.,1.,0.));
#7366=DIRECTION('ref_axis',(1.,0.,0.));
#7367=DIRECTION('',(0.,1.,0.));
#7368=DIRECTION('center_axis',(0.,-1.,0.));
#7369=DIRECTION('ref_axis',(1.,0.,0.));
#7370=DIRECTION('center_axis',(0.,1.,0.));
#7371=DIRECTION('ref_axis',(1.,0.,0.));
#7372=DIRECTION('center_axis',(0.,1.,0.));
#7373=DIRECTION('ref_axis',(1.,0.,0.));
#7374=DIRECTION('',(0.,1.,0.));
#7375=DIRECTION('center_axis',(0.,-1.,0.));
#7376=DIRECTION('ref_axis',(1.,0.,0.));
#7377=DIRECTION('center_axis',(0.,1.,0.));
#7378=DIRECTION('ref_axis',(1.,0.,0.));
#7379=DIRECTION('center_axis',(0.,1.,0.));
#7380=DIRECTION('ref_axis',(1.,0.,0.));
#7381=DIRECTION('',(0.,1.,0.));
#7382=DIRECTION('center_axis',(0.,-1.,0.));
#7383=DIRECTION('ref_axis',(1.,0.,0.));
#7384=DIRECTION('center_axis',(0.,1.,0.));
#7385=DIRECTION('ref_axis',(1.,0.,0.));
#7386=DIRECTION('center_axis',(0.,1.,0.));
#7387=DIRECTION('ref_axis',(1.,0.,0.));
#7388=DIRECTION('',(0.,1.,0.));
#7389=DIRECTION('center_axis',(0.,-1.,0.));
#7390=DIRECTION('ref_axis',(1.,0.,0.));
#7391=DIRECTION('center_axis',(0.,0.,1.));
#7392=DIRECTION('ref_axis',(0.707106781186548,0.707106781186548,0.));
#7393=DIRECTION('',(0.,0.,-1.));
#7394=DIRECTION('center_axis',(0.382683432365099,-8.20569863179165E-15,
0.923879532511283));
#7395=DIRECTION('ref_axis',(0.923879532511283,-1.98103089256172E-14,-0.382683432365098));
#7396=DIRECTION('',(0.,0.,1.));
#7397=DIRECTION('center_axis',(0.382683432365092,-1.98103089256178E-14,
-0.923879532511286));
#7398=DIRECTION('ref_axis',(-0.923879532511286,4.78263164830271E-14,-0.382683432365092));
#7399=DIRECTION('center_axis',(0.707106781186548,0.,0.707106781186548));
#7400=DIRECTION('ref_axis',(0.499999999999999,0.707106781186545,-0.500000000000005));
#7401=DIRECTION('',(-0.707106781186548,0.,-0.707106781186548));
#7402=DIRECTION('center_axis',(0.923879532511283,0.,0.382683432365099));
#7403=DIRECTION('ref_axis',(0.382683432365099,0.,-0.923879532511283));
#7404=DIRECTION('',(0.707106781186548,0.,0.707106781186548));
#7405=DIRECTION('center_axis',(1.,0.,0.));
#7406=DIRECTION('ref_axis',(0.,0.707106781186548,-0.707106781186548));
#7407=DIRECTION('',(-1.,0.,0.));
#7408=DIRECTION('center_axis',(0.923879532511286,1.69945583101724E-15,-0.382683432365092));
#7409=DIRECTION('ref_axis',(-0.382683432365092,4.10284931589584E-15,-0.923879532511286));
#7410=DIRECTION('',(1.,0.,0.));
#7411=DIRECTION('center_axis',(0.707106781186548,0.,-0.707106781186548));
#7412=DIRECTION('ref_axis',(-0.5,0.707106781186547,-0.5));
#7413=DIRECTION('',(-0.707106781186548,0.,0.707106781186548));
#7414=DIRECTION('center_axis',(0.382683432365092,0.,-0.923879532511286));
#7415=DIRECTION('ref_axis',(-0.923879532511286,0.,-0.382683432365091));
#7416=DIRECTION('',(0.707106781186548,0.,-0.707106781186548));
#7417=DIRECTION('center_axis',(0.,0.,-1.));
#7418=DIRECTION('ref_axis',(-0.707106781186548,0.707106781186548,0.));
#7419=DIRECTION('',(0.,0.,-1.));
#7420=DIRECTION('',(0.,0.,1.));
#7421=DIRECTION('center_axis',(-0.382683432365106,0.,-0.92387953251128));
#7422=DIRECTION('ref_axis',(-0.92387953251128,0.,0.382683432365106));
#7423=DIRECTION('center_axis',(-0.707106781186548,0.,-0.707106781186548));
#7424=DIRECTION('ref_axis',(-0.5,0.707106781186547,0.5));
#7425=DIRECTION('',(-0.707106781186548,0.,-0.707106781186548));
#7426=DIRECTION('',(0.707106781186548,0.,0.707106781186548));
#7427=DIRECTION('center_axis',(-0.923879532511291,0.,-0.382683432365079));
#7428=DIRECTION('ref_axis',(-0.382683432365079,0.,0.923879532511291));
#7429=DIRECTION('center_axis',(-1.,0.,0.));
#7430=DIRECTION('ref_axis',(0.,0.707106781186541,0.707106781186554));
#7431=DIRECTION('',(-1.,0.,0.));
#7432=DIRECTION('',(1.,0.,0.));
#7433=DIRECTION('center_axis',(-0.923879532511291,0.,0.382683432365079));
#7434=DIRECTION('ref_axis',(0.382683432365079,0.,0.923879532511291));
#7435=DIRECTION('center_axis',(-0.707106781186548,0.,0.707106781186548));
#7436=DIRECTION('ref_axis',(0.5,0.707106781186547,0.5));
#7437=DIRECTION('',(0.707106781186548,0.,-0.707106781186548));
#7438=DIRECTION('',(-0.707106781186548,0.,0.707106781186548));
#7439=DIRECTION('center_axis',(-0.707106781186548,0.,-0.707106781186548));
#7440=DIRECTION('ref_axis',(-0.707106781186548,0.,0.707106781186548));
#7441=DIRECTION('',(0.,-1.,0.));
#7442=DIRECTION('',(0.707106781186548,0.,-0.707106781186548));
#7443=DIRECTION('',(0.,1.,0.));
#7444=DIRECTION('center_axis',(0.,0.,-1.));
#7445=DIRECTION('ref_axis',(1.,0.,0.));
#7446=DIRECTION('',(0.,1.,0.));
#7447=DIRECTION('',(1.,0.,0.));
#7448=DIRECTION('center_axis',(0.707106781186548,0.,-0.707106781186548));
#7449=DIRECTION('ref_axis',(-0.707106781186548,0.,-0.707106781186548));
#7450=DIRECTION('',(0.,-1.,0.));
#7451=DIRECTION('',(0.707106781186548,0.,0.707106781186548));
#7452=DIRECTION('center_axis',(1.,0.,0.));
#7453=DIRECTION('ref_axis',(0.,0.,1.));
#7454=DIRECTION('',(0.,1.,0.));
#7455=DIRECTION('',(0.,0.,1.));
#7456=DIRECTION('center_axis',(0.,-1.,0.));
#7457=DIRECTION('ref_axis',(-1.,0.,0.));
#7458=DIRECTION('center_axis',(0.,0.,1.));
#7459=DIRECTION('ref_axis',(0.707106781186548,-0.707106781186548,0.));
#7460=DIRECTION('',(0.,0.,-1.));
#7461=DIRECTION('center_axis',(0.382683432365099,8.20569863179165E-15,0.923879532511283));
#7462=DIRECTION('ref_axis',(0.923879532511283,1.98103089256172E-14,-0.382683432365098));
#7463=DIRECTION('center_axis',(-0.382683432365106,1.64113972635832E-14,
0.92387953251128));
#7464=DIRECTION('ref_axis',(-0.92387953251128,-3.96206178512373E-14,-0.382683432365105));
#7465=DIRECTION('center_axis',(-0.707106781186548,0.,-0.707106781186548));
#7466=DIRECTION('ref_axis',(0.499999999999999,-0.707106781186545,-0.500000000000005));
#7467=DIRECTION('',(-0.707106781186548,0.,-0.707106781186548));
#7468=DIRECTION('center_axis',(0.923879532511284,0.,0.382683432365097));
#7469=DIRECTION('ref_axis',(-0.382683432365097,0.,0.923879532511284));
#7470=DIRECTION('center_axis',(1.,0.,0.));
#7471=DIRECTION('ref_axis',(0.,-0.707106781186544,-0.707106781186551));
#7472=DIRECTION('',(-1.,0.,0.));
#7473=DIRECTION('center_axis',(0.923879532511287,0.,-0.38268343236509));
#7474=DIRECTION('ref_axis',(-0.38268343236509,0.,-0.923879532511287));
#7475=DIRECTION('center_axis',(-0.707106781186548,0.,0.707106781186548));
#7476=DIRECTION('ref_axis',(-0.5,-0.707106781186547,-0.5));
#7477=DIRECTION('',(-0.707106781186548,0.,0.707106781186548));
#7478=DIRECTION('center_axis',(0.382683432365092,0.,-0.923879532511286));
#7479=DIRECTION('ref_axis',(0.923879532511286,0.,0.382683432365091));
#7480=DIRECTION('center_axis',(0.,0.,-1.));
#7481=DIRECTION('ref_axis',(-0.707106781186548,-0.707106781186548,0.));
#7482=DIRECTION('',(0.,0.,-1.));
#7483=DIRECTION('',(0.,0.,1.));
#7484=DIRECTION('center_axis',(-0.382683432365106,0.,-0.92387953251128));
#7485=DIRECTION('ref_axis',(-0.92387953251128,0.,0.382683432365106));
#7486=DIRECTION('center_axis',(0.707106781186548,0.,0.707106781186548));
#7487=DIRECTION('ref_axis',(-0.5,-0.707106781186547,0.5));
#7488=DIRECTION('',(-0.707106781186548,0.,-0.707106781186548));
#7489=DIRECTION('',(0.707106781186548,0.,0.707106781186548));
#7490=DIRECTION('center_axis',(-0.923879532511283,0.,-0.382683432365099));
#7491=DIRECTION('ref_axis',(0.382683432365099,0.,-0.923879532511283));
#7492=DIRECTION('center_axis',(-1.,0.,0.));
#7493=DIRECTION('ref_axis',(0.,-0.707106781186554,0.707106781186541));
#7494=DIRECTION('',(-1.,0.,0.));
#7495=DIRECTION('',(1.,0.,0.));
#7496=DIRECTION('center_axis',(-0.923879532511283,0.,0.382683432365099));
#7497=DIRECTION('ref_axis',(0.382683432365099,0.,0.923879532511283));
#7498=DIRECTION('center_axis',(0.707106781186548,0.,-0.707106781186548));
#7499=DIRECTION('ref_axis',(0.5,-0.707106781186547,0.5));
#7500=DIRECTION('',(-0.707106781186548,0.,0.707106781186548));
#7501=DIRECTION('',(0.707106781186548,0.,-0.707106781186548));
#7502=DIRECTION('center_axis',(-0.707106781186548,0.,0.707106781186548));
#7503=DIRECTION('ref_axis',(0.707106781186548,0.,0.707106781186548));
#7504=DIRECTION('',(0.,-1.,0.));
#7505=DIRECTION('',(0.,1.,0.));
#7506=DIRECTION('center_axis',(0.,0.,1.));
#7507=DIRECTION('ref_axis',(-1.,0.,0.));
#7508=DIRECTION('',(0.,-1.,0.));
#7509=DIRECTION('center_axis',(0.707106781186548,0.,0.707106781186548));
#7510=DIRECTION('ref_axis',(0.707106781186548,0.,-0.707106781186548));
#7511=DIRECTION('center_axis',(0.,-1.,0.));
#7512=DIRECTION('ref_axis',(0.,0.,-1.));
#7513=DIRECTION('center_axis',(-1.,0.,0.));
#7514=DIRECTION('ref_axis',(0.,0.,-1.));
#7515=DIRECTION('axis',(0.,0.,1.));
#7516=DIRECTION('refdir',(1.,0.,0.));
#7517=DIRECTION('center_axis',(0.,1.,0.));
#7518=DIRECTION('ref_axis',(1.,0.,0.));
#7519=DIRECTION('center_axis',(0.,1.,0.));
#7520=DIRECTION('ref_axis',(1.,0.,0.));
#7521=DIRECTION('',(0.,1.,0.));
#7522=DIRECTION('center_axis',(0.,-1.,0.));
#7523=DIRECTION('ref_axis',(1.,0.,0.));
#7524=DIRECTION('center_axis',(0.,1.,0.));
#7525=DIRECTION('ref_axis',(1.,0.,0.));
#7526=DIRECTION('center_axis',(0.,1.,0.));
#7527=DIRECTION('ref_axis',(1.,0.,0.));
#7528=DIRECTION('',(0.,1.,0.));
#7529=DIRECTION('center_axis',(0.,-1.,0.));
#7530=DIRECTION('ref_axis',(1.,0.,0.));
#7531=DIRECTION('center_axis',(0.,0.,-1.));
#7532=DIRECTION('ref_axis',(-1.,0.,0.));
#7533=DIRECTION('',(-1.,0.,0.));
#7534=DIRECTION('',(-0.268631512041369,0.963243017487471,0.));
#7535=DIRECTION('',(-1.,0.,0.));
#7536=DIRECTION('',(0.,1.,0.));
#7537=DIRECTION('',(1.,0.,0.));
#7538=DIRECTION('',(0.,-1.,0.));
#7539=DIRECTION('',(-1.,0.,0.));
#7540=DIRECTION('',(-0.268631512041369,-0.963243017487471,0.));
#7541=DIRECTION('center_axis',(-0.963243017487471,-0.268631512041369,0.));
#7542=DIRECTION('ref_axis',(0.268631512041369,-0.963243017487471,0.));
#7543=DIRECTION('',(0.,0.,1.));
#7544=DIRECTION('',(0.268631512041369,-0.963243017487471,0.));
#7545=DIRECTION('',(0.,0.,1.));
#7546=DIRECTION('center_axis',(0.,-1.,0.));
#7547=DIRECTION('ref_axis',(1.,0.,0.));
#7548=DIRECTION('',(1.,0.,0.));
#7549=DIRECTION('',(0.,0.,1.));
#7550=DIRECTION('center_axis',(-1.,0.,0.));
#7551=DIRECTION('ref_axis',(0.,-1.,0.));
#7552=DIRECTION('',(0.,-1.,0.));
#7553=DIRECTION('',(0.,0.,1.));
#7554=DIRECTION('center_axis',(0.,1.,0.));
#7555=DIRECTION('ref_axis',(-1.,0.,0.));
#7556=DIRECTION('',(-1.,0.,0.));
#7557=DIRECTION('',(0.,0.,1.));
#7558=DIRECTION('center_axis',(1.,0.,0.));
#7559=DIRECTION('ref_axis',(0.,1.,0.));
#7560=DIRECTION('',(0.,1.,0.));
#7561=DIRECTION('',(0.,0.,1.));
#7562=DIRECTION('center_axis',(0.,-1.,0.));
#7563=DIRECTION('ref_axis',(1.,0.,0.));
#7564=DIRECTION('',(1.,0.,0.));
#7565=DIRECTION('',(0.,0.,1.));
#7566=DIRECTION('center_axis',(0.963243017487471,-0.268631512041369,0.));
#7567=DIRECTION('ref_axis',(0.268631512041369,0.963243017487471,0.));
#7568=DIRECTION('',(0.268631512041369,0.963243017487471,0.));
#7569=DIRECTION('',(0.,0.,1.));
#7570=DIRECTION('center_axis',(0.,-1.,0.));
#7571=DIRECTION('ref_axis',(1.,0.,0.));
#7572=DIRECTION('',(1.,0.,0.));
#7573=DIRECTION('center_axis',(0.,0.,1.));
#7574=DIRECTION('ref_axis',(1.,0.,0.));
#7575=DIRECTION('axis',(0.,0.,1.));
#7576=DIRECTION('refdir',(1.,0.,0.));
#7577=DIRECTION('center_axis',(0.,0.,-1.));
#7578=DIRECTION('ref_axis',(-1.,0.,0.));
#7579=DIRECTION('center_axis',(0.,0.,-1.));
#7580=DIRECTION('ref_axis',(-1.,0.,0.));
#7581=DIRECTION('',(0.,0.,-1.));
#7582=DIRECTION('center_axis',(0.,0.,-1.));
#7583=DIRECTION('ref_axis',(-1.,0.,0.));
#7584=DIRECTION('center_axis',(0.,0.,1.));
#7585=DIRECTION('ref_axis',(-1.,0.,0.));
#7586=DIRECTION('center_axis',(0.,0.,-1.));
#7587=DIRECTION('ref_axis',(-1.,0.,0.));
#7588=DIRECTION('center_axis',(0.,0.,-1.));
#7589=DIRECTION('ref_axis',(-1.,0.,0.));
#7590=DIRECTION('',(0.,0.,-1.));
#7591=DIRECTION('center_axis',(0.,0.,-1.));
#7592=DIRECTION('ref_axis',(-1.,0.,0.));
#7593=DIRECTION('center_axis',(0.,0.,1.));
#7594=DIRECTION('ref_axis',(-1.,0.,0.));
#7595=DIRECTION('center_axis',(0.,0.,-1.));
#7596=DIRECTION('ref_axis',(-1.,0.,0.));
#7597=DIRECTION('center_axis',(0.,0.,-1.));
#7598=DIRECTION('ref_axis',(-1.,0.,0.));
#7599=DIRECTION('',(0.,0.,-1.));
#7600=DIRECTION('center_axis',(0.,0.,-1.));
#7601=DIRECTION('ref_axis',(-1.,0.,0.));
#7602=DIRECTION('center_axis',(0.,0.,1.));
#7603=DIRECTION('ref_axis',(-1.,0.,0.));
#7604=DIRECTION('center_axis',(1.,0.,0.));
#7605=DIRECTION('ref_axis',(0.,-0.707106781186557,0.707106781186538));
#7606=DIRECTION('',(-1.,0.,0.));
#7607=DIRECTION('center_axis',(0.707106781186548,-0.707106781186548,0.));
#7608=DIRECTION('ref_axis',(-0.707106781186548,-0.707106781186548,0.));
#7609=DIRECTION('',(1.,0.,0.));
#7610=DIRECTION('center_axis',(-0.707106781186548,-0.707106781186547,-1.5700924586838E-15));
#7611=DIRECTION('ref_axis',(-0.707106781186547,0.707106781186548,1.5700924586838E-15));
#7612=DIRECTION('center_axis',(0.,1.,0.));
#7613=DIRECTION('ref_axis',(-0.707106781186549,0.,0.707106781186546));
#7614=DIRECTION('',(0.,-1.,0.));
#7615=DIRECTION('',(0.,1.,0.));
#7616=DIRECTION('center_axis',(-0.707106781186549,-0.707106781186546,0.));
#7617=DIRECTION('ref_axis',(0.707106781186546,-0.707106781186549,0.));
#7618=DIRECTION('center_axis',(0.,1.,0.));
#7619=DIRECTION('ref_axis',(0.707106781186549,0.,0.707106781186546));
#7620=DIRECTION('',(0.,-1.,0.));
#7621=DIRECTION('',(0.,1.,0.));
#7622=DIRECTION('center_axis',(0.707106781186549,-0.707106781186546,-1.57009245868378E-15));
#7623=DIRECTION('ref_axis',(-0.707106781186546,-0.707106781186549,1.57009245868378E-15));
#7624=DIRECTION('center_axis',(1.,0.,0.));
#7625=DIRECTION('ref_axis',(0.,0.707106781186551,0.707106781186544));
#7626=DIRECTION('',(-1.,0.,0.));
#7627=DIRECTION('',(1.,0.,0.));
#7628=DIRECTION('center_axis',(1.,0.,0.));
#7629=DIRECTION('ref_axis',(0.,0.,-1.));
#7630=DIRECTION('',(0.,0.,-1.));
#7631=DIRECTION('center_axis',(1.,0.,0.));
#7632=DIRECTION('ref_axis',(0.,-0.707106781186554,0.707106781186541));
#7633=DIRECTION('',(0.,-1.,0.));
#7634=DIRECTION('center_axis',(1.,0.,0.));
#7635=DIRECTION('ref_axis',(0.,0.707106781186541,0.707106781186554));
#7636=DIRECTION('',(0.,0.,-1.));
#7637=DIRECTION('center_axis',(0.,-1.,0.));
#7638=DIRECTION('ref_axis',(0.,0.,-1.));
#7639=DIRECTION('',(0.,0.,1.));
#7640=DIRECTION('',(1.,0.,0.));
#7641=DIRECTION('',(0.707106781186548,0.,0.707106781186548));
#7642=DIRECTION('',(0.,0.,1.));
#7643=DIRECTION('',(-0.707106781186548,0.,0.707106781186548));
#7644=DIRECTION('',(-1.,0.,0.));
#7645=DIRECTION('',(-0.707106781186548,0.,-0.707106781186548));
#7646=DIRECTION('',(0.,0.,-1.));
#7647=DIRECTION('',(0.707106781186548,0.,-0.707106781186548));
#7648=DIRECTION('',(1.,0.,0.));
#7649=DIRECTION('center_axis',(0.,0.,1.));
#7650=DIRECTION('ref_axis',(1.,0.,0.));
#7651=DIRECTION('center_axis',(-1.,0.,0.));
#7652=DIRECTION('ref_axis',(0.,0.,1.));
#7653=DIRECTION('',(0.,0.,1.));
#7654=DIRECTION('center_axis',(-1.,0.,0.));
#7655=DIRECTION('ref_axis',(0.,0.707106781186541,0.707106781186554));
#7656=DIRECTION('',(0.,1.,0.));
#7657=DIRECTION('center_axis',(-1.,0.,0.));
#7658=DIRECTION('ref_axis',(0.,-0.707106781186554,0.707106781186541));
#7659=DIRECTION('center_axis',(0.,-1.,0.));
#7660=DIRECTION('ref_axis',(-1.,0.,0.));
#7661=DIRECTION('',(-1.,0.,0.));
#7662=DIRECTION('',(-0.707106781186548,0.,0.707106781186548));
#7663=DIRECTION('',(0.,0.,1.));
#7664=DIRECTION('',(0.707106781186548,0.,0.707106781186548));
#7665=DIRECTION('',(1.,0.,0.));
#7666=DIRECTION('',(0.707106781186548,0.,-0.707106781186548));
#7667=DIRECTION('',(0.,0.,-1.));
#7668=DIRECTION('',(-0.707106781186548,0.,-0.707106781186548));
#7669=DIRECTION('',(-1.,0.,0.));
#7670=DIRECTION('center_axis',(-1.,0.,0.));
#7671=DIRECTION('ref_axis',(0.,0.707106781186541,0.707106781186554));
#7672=DIRECTION('',(1.,0.,0.));
#7673=DIRECTION('center_axis',(-0.923879532511291,0.,0.382683432365079));
#7674=DIRECTION('ref_axis',(0.382683432365079,0.,0.923879532511291));
#7675=DIRECTION('center_axis',(-1.,0.,0.));
#7676=DIRECTION('ref_axis',(0.,0.707106781186541,0.707106781186554));
#7677=DIRECTION('center_axis',(-0.923879532511291,0.,-0.382683432365079));
#7678=DIRECTION('ref_axis',(-0.382683432365079,0.,0.923879532511291));
#7679=DIRECTION('',(1.,0.,0.));
#7680=DIRECTION('center_axis',(0.,0.,1.));
#7681=DIRECTION('ref_axis',(-1.,0.,0.));
#7682=DIRECTION('',(-1.,0.,0.));
#7683=DIRECTION('',(0.,-1.,0.));
#7684=DIRECTION('center_axis',(-1.,0.,0.));
#7685=DIRECTION('ref_axis',(0.,-0.707106781186554,0.707106781186541));
#7686=DIRECTION('center_axis',(-0.923879532511283,0.,0.382683432365099));
#7687=DIRECTION('ref_axis',(0.382683432365099,0.,0.923879532511283));
#7688=DIRECTION('center_axis',(0.,0.,1.));
#7689=DIRECTION('ref_axis',(0.707106781186548,0.707106781186548,0.));
#7690=DIRECTION('',(0.,0.,-1.));
#7691=DIRECTION('center_axis',(0.382683432365099,-8.20569863179165E-15,
0.923879532511283));
#7692=DIRECTION('ref_axis',(0.923879532511283,-1.98103089256172E-14,-0.382683432365098));
#7693=DIRECTION('center_axis',(0.382683432365092,-1.98103089256178E-14,
-0.923879532511286));
#7694=DIRECTION('ref_axis',(-0.923879532511286,4.78263164830271E-14,-0.382683432365092));
#7695=DIRECTION('center_axis',(0.707106781186548,0.,0.707106781186548));
#7696=DIRECTION('ref_axis',(0.499999999999999,0.707106781186545,-0.500000000000005));
#7697=DIRECTION('',(-0.707106781186548,0.,-0.707106781186548));
#7698=DIRECTION('center_axis',(0.923879532511283,0.,0.382683432365099));
#7699=DIRECTION('ref_axis',(0.382683432365099,0.,-0.923879532511283));
#7700=DIRECTION('center_axis',(1.,0.,0.));
#7701=DIRECTION('ref_axis',(0.,0.707106781186548,-0.707106781186548));
#7702=DIRECTION('',(-1.,0.,0.));
#7703=DIRECTION('center_axis',(0.923879532511286,1.69945583101724E-15,-0.382683432365092));
#7704=DIRECTION('ref_axis',(-0.382683432365092,4.10284931589584E-15,-0.923879532511286));
#7705=DIRECTION('center_axis',(0.707106781186548,0.,-0.707106781186548));
#7706=DIRECTION('ref_axis',(-0.5,0.707106781186547,-0.5));
#7707=DIRECTION('',(-0.707106781186548,0.,0.707106781186548));
#7708=DIRECTION('center_axis',(0.382683432365092,0.,-0.923879532511286));
#7709=DIRECTION('ref_axis',(-0.923879532511286,0.,-0.382683432365091));
#7710=DIRECTION('center_axis',(0.,0.,-1.));
#7711=DIRECTION('ref_axis',(-0.707106781186548,0.707106781186548,0.));
#7712=DIRECTION('',(0.,0.,1.));
#7713=DIRECTION('center_axis',(-0.382683432365106,0.,-0.92387953251128));
#7714=DIRECTION('ref_axis',(-0.92387953251128,0.,0.382683432365106));
#7715=DIRECTION('center_axis',(-0.707106781186548,0.,-0.707106781186548));
#7716=DIRECTION('ref_axis',(-0.5,0.707106781186547,0.5));
#7717=DIRECTION('',(0.707106781186548,0.,0.707106781186548));
#7718=DIRECTION('center_axis',(-0.707106781186548,0.,0.707106781186548));
#7719=DIRECTION('ref_axis',(0.5,0.707106781186547,0.5));
#7720=DIRECTION('',(0.707106781186548,0.,-0.707106781186548));
#7721=DIRECTION('center_axis',(-0.707106781186548,0.,-0.707106781186548));
#7722=DIRECTION('ref_axis',(-0.707106781186548,0.,0.707106781186548));
#7723=DIRECTION('',(0.,-1.,0.));
#7724=DIRECTION('',(0.707106781186548,0.,-0.707106781186548));
#7725=DIRECTION('',(0.,1.,0.));
#7726=DIRECTION('center_axis',(0.,0.,-1.));
#7727=DIRECTION('ref_axis',(1.,0.,0.));
#7728=DIRECTION('',(0.,1.,0.));
#7729=DIRECTION('',(1.,0.,0.));
#7730=DIRECTION('center_axis',(0.707106781186548,0.,-0.707106781186548));
#7731=DIRECTION('ref_axis',(-0.707106781186548,0.,-0.707106781186548));
#7732=DIRECTION('',(0.,-1.,0.));
#7733=DIRECTION('',(0.707106781186548,0.,0.707106781186548));
#7734=DIRECTION('center_axis',(1.,0.,0.));
#7735=DIRECTION('ref_axis',(0.,0.,1.));
#7736=DIRECTION('',(0.,1.,0.));
#7737=DIRECTION('',(0.,0.,1.));
#7738=DIRECTION('center_axis',(0.,0.,1.));
#7739=DIRECTION('ref_axis',(0.707106781186548,-0.707106781186548,0.));
#7740=DIRECTION('center_axis',(0.382683432365099,8.20569863179165E-15,0.923879532511283));
#7741=DIRECTION('ref_axis',(0.923879532511283,1.98103089256172E-14,-0.382683432365098));
#7742=DIRECTION('center_axis',(-0.382683432365106,1.64113972635832E-14,
0.92387953251128));
#7743=DIRECTION('ref_axis',(-0.92387953251128,-3.96206178512373E-14,-0.382683432365105));
#7744=DIRECTION('center_axis',(-0.707106781186548,0.,-0.707106781186548));
#7745=DIRECTION('ref_axis',(0.499999999999999,-0.707106781186545,-0.500000000000005));
#7746=DIRECTION('center_axis',(0.923879532511284,0.,0.382683432365097));
#7747=DIRECTION('ref_axis',(-0.382683432365097,0.,0.923879532511284));
#7748=DIRECTION('center_axis',(1.,0.,0.));
#7749=DIRECTION('ref_axis',(0.,-0.707106781186544,-0.707106781186551));
#7750=DIRECTION('center_axis',(0.923879532511287,0.,-0.38268343236509));
#7751=DIRECTION('ref_axis',(-0.38268343236509,0.,-0.923879532511287));
#7752=DIRECTION('center_axis',(-0.707106781186548,0.,0.707106781186548));
#7753=DIRECTION('ref_axis',(-0.5,-0.707106781186547,-0.5));
#7754=DIRECTION('center_axis',(0.382683432365092,0.,-0.923879532511286));
#7755=DIRECTION('ref_axis',(0.923879532511286,0.,0.382683432365091));
#7756=DIRECTION('center_axis',(0.,0.,-1.));
#7757=DIRECTION('ref_axis',(-0.707106781186548,-0.707106781186548,0.));
#7758=DIRECTION('',(0.,0.,-1.));
#7759=DIRECTION('center_axis',(-0.382683432365106,0.,-0.92387953251128));
#7760=DIRECTION('ref_axis',(-0.92387953251128,0.,0.382683432365106));
#7761=DIRECTION('center_axis',(0.707106781186548,0.,0.707106781186548));
#7762=DIRECTION('ref_axis',(-0.5,-0.707106781186547,0.5));
#7763=DIRECTION('',(-0.707106781186548,0.,-0.707106781186548));
#7764=DIRECTION('center_axis',(-0.923879532511283,0.,-0.382683432365099));
#7765=DIRECTION('ref_axis',(0.382683432365099,0.,-0.923879532511283));
#7766=DIRECTION('center_axis',(-1.,0.,0.));
#7767=DIRECTION('ref_axis',(0.,-0.707106781186554,0.707106781186541));
#7768=DIRECTION('',(-1.,0.,0.));
#7769=DIRECTION('center_axis',(0.707106781186548,0.,-0.707106781186548));
#7770=DIRECTION('ref_axis',(0.5,-0.707106781186547,0.5));
#7771=DIRECTION('',(-0.707106781186548,0.,0.707106781186548));
#7772=DIRECTION('center_axis',(-0.707106781186548,0.,0.707106781186548));
#7773=DIRECTION('ref_axis',(0.707106781186548,0.,0.707106781186548));
#7774=DIRECTION('',(0.,-1.,0.));
#7775=DIRECTION('',(0.,1.,0.));
#7776=DIRECTION('center_axis',(0.,0.,1.));
#7777=DIRECTION('ref_axis',(-1.,0.,0.));
#7778=DIRECTION('center_axis',(0.707106781186548,0.,0.707106781186548));
#7779=DIRECTION('ref_axis',(0.707106781186548,0.,-0.707106781186548));
#7780=DIRECTION('center_axis',(-1.,0.,0.));
#7781=DIRECTION('ref_axis',(0.,0.,-1.));
#7782=DIRECTION('axis',(0.,0.,1.));
#7783=DIRECTION('refdir',(1.,0.,0.));
#7784=DIRECTION('center_axis',(0.,0.,-1.));
#7785=DIRECTION('ref_axis',(-1.,0.,0.));
#7786=DIRECTION('center_axis',(0.,0.,-1.));
#7787=DIRECTION('ref_axis',(-1.,0.,0.));
#7788=DIRECTION('',(0.,0.,-1.));
#7789=DIRECTION('center_axis',(0.,0.,1.));
#7790=DIRECTION('ref_axis',(-1.,0.,0.));
#7791=DIRECTION('center_axis',(0.,0.,-1.));
#7792=DIRECTION('ref_axis',(-1.,0.,0.));
#7793=DIRECTION('center_axis',(0.,0.,-1.));
#7794=DIRECTION('ref_axis',(-1.,0.,0.));
#7795=DIRECTION('',(0.,0.,-1.));
#7796=DIRECTION('center_axis',(0.,0.,1.));
#7797=DIRECTION('ref_axis',(-1.,0.,0.));
#7798=DIRECTION('center_axis',(0.,0.,-1.));
#7799=DIRECTION('ref_axis',(-1.,0.,0.));
#7800=DIRECTION('center_axis',(0.,0.,-1.));
#7801=DIRECTION('ref_axis',(-1.,0.,0.));
#7802=DIRECTION('',(0.,0.,-1.));
#7803=DIRECTION('center_axis',(0.,0.,1.));
#7804=DIRECTION('ref_axis',(-1.,0.,0.));
#7805=DIRECTION('center_axis',(0.,0.,-1.));
#7806=DIRECTION('ref_axis',(-1.,0.,0.));
#7807=DIRECTION('center_axis',(0.,0.,-1.));
#7808=DIRECTION('ref_axis',(-1.,0.,0.));
#7809=DIRECTION('',(0.,0.,-1.));
#7810=DIRECTION('center_axis',(0.,0.,1.));
#7811=DIRECTION('ref_axis',(-1.,0.,0.));
#7812=DIRECTION('center_axis',(-1.,0.,0.));
#7813=DIRECTION('ref_axis',(0.,-0.707106781186548,-0.707106781186548));
#7814=DIRECTION('',(1.,0.,0.));
#7815=DIRECTION('center_axis',(-0.923879532511283,-0.382683432365099,4.10284931589583E-15));
#7816=DIRECTION('ref_axis',(0.382683432365098,-0.923879532511283,9.90515446280861E-15));
#7817=DIRECTION('',(-1.,0.,0.));
#7818=DIRECTION('center_axis',(-0.923879532511286,0.382683432365092,0.));
#7819=DIRECTION('ref_axis',(0.382683432365091,0.923879532511286,0.));
#7820=DIRECTION('center_axis',(0.,1.,0.));
#7821=DIRECTION('ref_axis',(0.707106781186551,0.,-0.707106781186544));
#7822=DIRECTION('',(0.,1.,0.));
#7823=DIRECTION('center_axis',(-0.382683432365083,-0.92387953251129,0.));
#7824=DIRECTION('ref_axis',(0.923879532511289,-0.382683432365083,0.));
#7825=DIRECTION('',(0.,-1.,0.));
#7826=DIRECTION('center_axis',(0.382683432365097,0.923879532511284,8.49727915508632E-16));
#7827=DIRECTION('ref_axis',(0.923879532511284,-0.382683432365097,2.05142465794791E-15));
#7828=DIRECTION('center_axis',(0.707106781186548,0.707106781186548,0.));
#7829=DIRECTION('ref_axis',(0.499999999999996,-0.500000000000002,-0.707106781186549));
#7830=DIRECTION('',(0.707106781186548,0.707106781186548,0.));
#7831=DIRECTION('center_axis',(-0.92387953251129,-0.382683432365082,0.));
#7832=DIRECTION('ref_axis',(0.382683432365082,-0.92387953251129,0.));
#7833=DIRECTION('',(-0.707106781186548,-0.707106781186548,0.));
#7834=DIRECTION('center_axis',(0.,1.,0.));
#7835=DIRECTION('ref_axis',(0.707106781186548,0.,-0.707106781186548));
#7836=DIRECTION('',(0.,-1.,0.));
#7837=DIRECTION('center_axis',(0.382683432365093,0.923879532511285,0.));
#7838=DIRECTION('ref_axis',(0.923879532511285,-0.382683432365093,0.));
#7839=DIRECTION('',(0.,1.,0.));
#7840=DIRECTION('center_axis',(0.382683432365092,-0.923879532511286,0.));
#7841=DIRECTION('ref_axis',(-0.923879532511286,-0.382683432365092,0.));
#7842=DIRECTION('center_axis',(1.,4.56509835347174E-16,0.));
#7843=DIRECTION('ref_axis',(0.,-0.707106781186551,-0.707106781186544));
#7844=DIRECTION('',(1.,4.56509835347174E-16,0.));
#7845=DIRECTION('center_axis',(-0.923879532511287,-0.38268343236509,0.));
#7846=DIRECTION('ref_axis',(-0.38268343236509,0.923879532511287,0.));
#7847=DIRECTION('',(-1.,-4.56509835347174E-16,0.));
#7848=DIRECTION('center_axis',(0.707106781186548,0.707106781186547,0.));
#7849=DIRECTION('ref_axis',(0.5,-0.5,-0.707106781186547));
#7850=DIRECTION('',(-0.707106781186548,-0.707106781186547,0.));
#7851=DIRECTION('',(0.707106781186548,0.707106781186547,0.));
#7852=DIRECTION('center_axis',(-0.707106781186548,0.707106781186548,0.));
#7853=DIRECTION('ref_axis',(0.5,0.5,-0.707106781186547));
#7854=DIRECTION('',(0.707106781186548,-0.707106781186548,0.));
#7855=DIRECTION('',(-0.707106781186548,0.707106781186548,0.));
#7856=DIRECTION('center_axis',(0.923879532511286,-0.382683432365092,0.));
#7857=DIRECTION('ref_axis',(-0.382683432365091,-0.923879532511286,0.));
#7858=DIRECTION('center_axis',(-1.,0.,0.));
#7859=DIRECTION('ref_axis',(0.,0.707106781186548,-0.707106781186548));
#7860=DIRECTION('',(1.,0.,0.));
#7861=DIRECTION('',(-1.,0.,0.));
#7862=DIRECTION('center_axis',(0.923879532511286,0.382683432365092,0.));
#7863=DIRECTION('ref_axis',(0.382683432365092,-0.923879532511286,0.));
#7864=DIRECTION('center_axis',(0.707106781186548,0.707106781186548,0.));
#7865=DIRECTION('ref_axis',(0.5,-0.5,-0.707106781186547));
#7866=DIRECTION('',(0.707106781186548,0.707106781186548,0.));
#7867=DIRECTION('',(-0.707106781186548,-0.707106781186548,0.));
#7868=DIRECTION('center_axis',(-0.707106781186548,-0.707106781186548,0.));
#7869=DIRECTION('ref_axis',(-0.5,0.5,-0.707106781186547));
#7870=DIRECTION('',(0.707106781186548,0.707106781186548,0.));
#7871=DIRECTION('',(-0.707106781186548,-0.707106781186548,0.));
#7872=DIRECTION('center_axis',(0.382683432365092,0.923879532511286,0.));
#7873=DIRECTION('ref_axis',(0.923879532511286,-0.382683432365091,0.));
#7874=DIRECTION('center_axis',(0.,-1.,0.));
#7875=DIRECTION('ref_axis',(-0.707106781186548,0.,-0.707106781186548));
#7876=DIRECTION('',(0.,1.,0.));
#7877=DIRECTION('',(0.,-1.,0.));
#7878=DIRECTION('center_axis',(-0.382683432365092,0.923879532511286,0.));
#7879=DIRECTION('ref_axis',(0.923879532511286,0.382683432365092,0.));
#7880=DIRECTION('center_axis',(0.707106781186548,-0.707106781186548,0.));
#7881=DIRECTION('ref_axis',(-0.5,-0.5,-0.707106781186547));
#7882=DIRECTION('',(-0.707106781186548,0.707106781186548,0.));
#7883=DIRECTION('',(0.707106781186548,-0.707106781186548,0.));
#7884=DIRECTION('center_axis',(0.707106781186548,-0.707106781186548,0.));
#7885=DIRECTION('ref_axis',(0.,0.,-1.));
#7886=DIRECTION('',(0.,0.,1.));
#7887=DIRECTION('',(0.707106781186548,0.707106781186548,0.));
#7888=DIRECTION('',(0.,0.,-1.));
#7889=DIRECTION('center_axis',(1.,0.,0.));
#7890=DIRECTION('ref_axis',(0.,1.,0.));
#7891=DIRECTION('',(0.,0.,1.));
#7892=DIRECTION('',(0.,1.,0.));
#7893=DIRECTION('center_axis',(0.707106781186548,-0.707106781186548,0.));
#7894=DIRECTION('ref_axis',(0.707106781186548,0.707106781186548,0.));
#7895=DIRECTION('',(0.,0.,1.));
#7896=DIRECTION('',(0.707106781186548,0.707106781186548,0.));
#7897=DIRECTION('center_axis',(4.56509835347174E-16,-1.,0.));
#7898=DIRECTION('ref_axis',(1.,4.56509835347174E-16,0.));
#7899=DIRECTION('',(0.,0.,-1.));
#7900=DIRECTION('',(1.,4.56509835347174E-16,0.));
#7901=DIRECTION('center_axis',(0.707106781186547,-0.707106781186548,0.));
#7902=DIRECTION('ref_axis',(0.,0.,-1.));
#7903=DIRECTION('',(0.,0.,1.));
#7904=DIRECTION('',(0.707106781186548,0.707106781186547,0.));
#7905=DIRECTION('center_axis',(1.,0.,0.));
#7906=DIRECTION('ref_axis',(0.,1.,0.));
#7907=DIRECTION('',(0.,0.,1.));
#7908=DIRECTION('',(0.,1.,0.));
#7909=DIRECTION('center_axis',(0.,0.,1.));
#7910=DIRECTION('ref_axis',(1.,0.,0.));
#7911=DIRECTION('center_axis',(0.707106781186548,-0.707106781186548,0.));
#7912=DIRECTION('ref_axis',(-0.500000000000005,-0.500000000000005,0.707106781186541));
#7913=DIRECTION('',(-0.707106781186548,0.707106781186548,0.));
#7914=DIRECTION('center_axis',(0.382683432365092,-0.923879532511286,0.));
#7915=DIRECTION('ref_axis',(-0.923879532511286,-0.382683432365092,0.));
#7916=DIRECTION('',(0.707106781186548,-0.707106781186548,0.));
#7917=DIRECTION('center_axis',(0.923879532511286,-0.382683432365092,0.));
#7918=DIRECTION('ref_axis',(-0.382683432365092,-0.923879532511286,0.));
#7919=DIRECTION('center_axis',(0.,-1.,0.));
#7920=DIRECTION('ref_axis',(-0.707106781186554,0.,0.707106781186541));
#7921=DIRECTION('',(0.,1.,0.));
#7922=DIRECTION('center_axis',(-0.382683432365092,-0.923879532511286,0.));
#7923=DIRECTION('ref_axis',(-0.923879532511286,0.382683432365092,0.));
#7924=DIRECTION('',(0.,-1.,0.));
#7925=DIRECTION('center_axis',(-0.707106781186548,-0.707106781186548,0.));
#7926=DIRECTION('ref_axis',(-0.500000000000005,0.500000000000005,0.707106781186541));
#7927=DIRECTION('',(0.707106781186548,0.707106781186548,0.));
#7928=DIRECTION('center_axis',(-0.923879532511286,-0.382683432365092,0.));
#7929=DIRECTION('ref_axis',(-0.382683432365092,0.923879532511286,0.));
#7930=DIRECTION('',(-0.707106781186548,-0.707106781186548,0.));
#7931=DIRECTION('center_axis',(-1.,0.,0.));
#7932=DIRECTION('ref_axis',(0.,0.707106781186554,0.707106781186541));
#7933=DIRECTION('',(1.,0.,0.));
#7934=DIRECTION('center_axis',(-0.923879532511286,0.382683432365092,0.));
#7935=DIRECTION('ref_axis',(0.382683432365092,0.923879532511286,0.));
#7936=DIRECTION('',(-1.,0.,0.));
#7937=DIRECTION('center_axis',(-0.707106781186548,0.707106781186548,0.));
#7938=DIRECTION('ref_axis',(0.500000000000005,0.500000000000005,0.707106781186541));
#7939=DIRECTION('',(0.707106781186548,-0.707106781186548,0.));
#7940=DIRECTION('center_axis',(-0.382683432365092,0.923879532511286,0.));
#7941=DIRECTION('ref_axis',(0.923879532511286,0.382683432365092,0.));
#7942=DIRECTION('',(-0.707106781186548,0.707106781186548,0.));
#7943=DIRECTION('center_axis',(0.,1.,0.));
#7944=DIRECTION('ref_axis',(0.707106781186554,0.,0.707106781186541));
#7945=DIRECTION('',(0.,-1.,0.));
#7946=DIRECTION('center_axis',(0.382683432365093,0.923879532511285,0.));
#7947=DIRECTION('ref_axis',(0.923879532511285,-0.382683432365093,0.));
#7948=DIRECTION('center_axis',(-0.707106781186548,-0.707106781186547,0.));
#7949=DIRECTION('ref_axis',(0.5,-0.5,0.707106781186547));
#7950=DIRECTION('',(-0.707106781186548,-0.707106781186547,0.));
#7951=DIRECTION('center_axis',(0.923879532511287,0.38268343236509,0.));
#7952=DIRECTION('ref_axis',(-0.38268343236509,0.923879532511287,0.));
#7953=DIRECTION('center_axis',(1.,4.56509835347174E-16,0.));
#7954=DIRECTION('ref_axis',(0.,-0.707106781186557,0.707106781186538));
#7955=DIRECTION('',(-1.,-4.56509835347174E-16,0.));
#7956=DIRECTION('center_axis',(0.92387953251129,0.382683432365082,0.));
#7957=DIRECTION('ref_axis',(-0.382683432365082,0.92387953251129,0.));
#7958=DIRECTION('center_axis',(0.707106781186548,0.707106781186548,0.));
#7959=DIRECTION('ref_axis',(0.500000000000005,-0.500000000000005,0.707106781186541));
#7960=DIRECTION('',(-0.707106781186548,-0.707106781186548,0.));
#7961=DIRECTION('center_axis',(0.382683432365087,0.923879532511288,0.));
#7962=DIRECTION('ref_axis',(-0.923879532511288,0.382683432365087,0.));
#7963=DIRECTION('center_axis',(0.,1.,0.));
#7964=DIRECTION('ref_axis',(0.707106781186557,0.,0.707106781186538));
#7965=DIRECTION('',(0.,-1.,0.));
#7966=DIRECTION('center_axis',(0.382683432365097,0.923879532511284,-8.4972791550864E-16));
#7967=DIRECTION('ref_axis',(0.923879532511284,-0.382683432365097,-2.05142465794793E-15));
#7968=DIRECTION('center_axis',(-0.707106781186548,-0.707106781186548,0.));
#7969=DIRECTION('ref_axis',(0.5,-0.5,0.707106781186547));
#7970=DIRECTION('',(-0.707106781186548,-0.707106781186548,0.));
#7971=DIRECTION('center_axis',(0.923879532511283,0.382683432365099,0.));
#7972=DIRECTION('ref_axis',(-0.382683432365099,0.923879532511283,0.));
#7973=DIRECTION('center_axis',(1.,0.,0.));
#7974=DIRECTION('ref_axis',(0.,-0.707106781186554,0.707106781186541));
#7975=DIRECTION('',(1.,0.,0.));
#7976=DIRECTION('',(-1.,0.,0.));
#7977=DIRECTION('center_axis',(0.,-1.,0.));
#7978=DIRECTION('ref_axis',(1.,0.,0.));
#7979=DIRECTION('',(0.,0.,1.));
#7980=DIRECTION('center_axis',(-0.707106781186548,-0.707106781186548,0.));
#7981=DIRECTION('ref_axis',(0.707106781186548,-0.707106781186548,0.));
#7982=DIRECTION('',(0.,0.,1.));
#7983=DIRECTION('center_axis',(0.,0.,1.));
#7984=DIRECTION('ref_axis',(1.,0.,0.));
#7985=DIRECTION('center_axis',(-1.,0.,0.));
#7986=DIRECTION('ref_axis',(0.,-1.,0.));
#7987=DIRECTION('',(0.,0.,1.));
#7988=DIRECTION('center_axis',(-0.707106781186548,0.707106781186548,0.));
#7989=DIRECTION('ref_axis',(-0.707106781186548,-0.707106781186548,0.));
#7990=DIRECTION('',(0.,0.,1.));
#7991=DIRECTION('center_axis',(0.,1.,0.));
#7992=DIRECTION('ref_axis',(-1.,0.,0.));
#7993=DIRECTION('',(0.,0.,1.));
#7994=DIRECTION('center_axis',(0.707106781186548,0.707106781186548,0.));
#7995=DIRECTION('ref_axis',(-0.707106781186548,0.707106781186548,0.));
#7996=DIRECTION('axis',(0.,0.,1.));
#7997=DIRECTION('refdir',(1.,0.,0.));
#7998=DIRECTION('center_axis',(0.,0.,-1.));
#7999=DIRECTION('ref_axis',(-1.,0.,0.));
#8000=DIRECTION('center_axis',(0.,0.,-1.));
#8001=DIRECTION('ref_axis',(-1.,0.,0.));
#8002=DIRECTION('',(0.,0.,-1.));
#8003=DIRECTION('center_axis',(0.,0.,1.));
#8004=DIRECTION('ref_axis',(-1.,0.,0.));
#8005=DIRECTION('center_axis',(0.,0.,-1.));
#8006=DIRECTION('ref_axis',(-1.,0.,0.));
#8007=DIRECTION('center_axis',(0.,0.,-1.));
#8008=DIRECTION('ref_axis',(-1.,0.,0.));
#8009=DIRECTION('',(0.,0.,-1.));
#8010=DIRECTION('center_axis',(0.,0.,1.));
#8011=DIRECTION('ref_axis',(-1.,0.,0.));
#8012=DIRECTION('center_axis',(0.,0.,-1.));
#8013=DIRECTION('ref_axis',(-1.,0.,0.));
#8014=DIRECTION('center_axis',(0.,0.,-1.));
#8015=DIRECTION('ref_axis',(-1.,0.,0.));
#8016=DIRECTION('',(0.,0.,-1.));
#8017=DIRECTION('center_axis',(0.,0.,1.));
#8018=DIRECTION('ref_axis',(-1.,0.,0.));
#8019=DIRECTION('center_axis',(0.,0.,-1.));
#8020=DIRECTION('ref_axis',(-1.,0.,0.));
#8021=DIRECTION('center_axis',(0.,0.,-1.));
#8022=DIRECTION('ref_axis',(-1.,0.,0.));
#8023=DIRECTION('',(0.,0.,-1.));
#8024=DIRECTION('center_axis',(0.,0.,1.));
#8025=DIRECTION('ref_axis',(-1.,0.,0.));
#8026=DIRECTION('center_axis',(-1.,0.,0.));
#8027=DIRECTION('ref_axis',(0.,-0.707106781186548,-0.707106781186548));
#8028=DIRECTION('',(1.,0.,0.));
#8029=DIRECTION('center_axis',(-0.923879532511283,-0.382683432365099,4.10284931589583E-15));
#8030=DIRECTION('ref_axis',(0.382683432365098,-0.923879532511283,9.90515446280861E-15));
#8031=DIRECTION('',(-1.,0.,0.));
#8032=DIRECTION('center_axis',(-0.923879532511286,0.382683432365092,0.));
#8033=DIRECTION('ref_axis',(0.382683432365091,0.923879532511286,0.));
#8034=DIRECTION('center_axis',(0.,1.,0.));
#8035=DIRECTION('ref_axis',(0.707106781186551,0.,-0.707106781186544));
#8036=DIRECTION('',(0.,1.,0.));
#8037=DIRECTION('center_axis',(-0.382683432365083,-0.92387953251129,0.));
#8038=DIRECTION('ref_axis',(0.923879532511289,-0.382683432365083,0.));
#8039=DIRECTION('',(0.,-1.,0.));
#8040=DIRECTION('center_axis',(0.382683432365097,0.923879532511284,8.49727915508632E-16));
#8041=DIRECTION('ref_axis',(0.923879532511284,-0.382683432365097,2.05142465794791E-15));
#8042=DIRECTION('center_axis',(0.707106781186548,0.707106781186548,0.));
#8043=DIRECTION('ref_axis',(0.499999999999996,-0.500000000000002,-0.707106781186549));
#8044=DIRECTION('',(0.707106781186548,0.707106781186548,0.));
#8045=DIRECTION('center_axis',(-0.92387953251129,-0.382683432365082,0.));
#8046=DIRECTION('ref_axis',(0.382683432365082,-0.92387953251129,0.));
#8047=DIRECTION('',(-0.707106781186548,-0.707106781186548,0.));
#8048=DIRECTION('center_axis',(0.,1.,0.));
#8049=DIRECTION('ref_axis',(0.707106781186548,0.,-0.707106781186548));
#8050=DIRECTION('',(0.,-1.,0.));
#8051=DIRECTION('center_axis',(0.382683432365093,0.923879532511285,0.));
#8052=DIRECTION('ref_axis',(0.923879532511285,-0.382683432365093,0.));
#8053=DIRECTION('',(0.,1.,0.));
#8054=DIRECTION('center_axis',(0.382683432365092,-0.923879532511286,0.));
#8055=DIRECTION('ref_axis',(-0.923879532511286,-0.382683432365092,0.));
#8056=DIRECTION('center_axis',(1.,4.56509835347174E-16,0.));
#8057=DIRECTION('ref_axis',(0.,-0.707106781186551,-0.707106781186544));
#8058=DIRECTION('',(1.,4.56509835347174E-16,0.));
#8059=DIRECTION('center_axis',(-0.923879532511287,-0.38268343236509,0.));
#8060=DIRECTION('ref_axis',(-0.38268343236509,0.923879532511287,0.));
#8061=DIRECTION('',(-1.,-4.56509835347174E-16,0.));
#8062=DIRECTION('center_axis',(0.707106781186548,0.707106781186547,0.));
#8063=DIRECTION('ref_axis',(0.5,-0.5,-0.707106781186547));
#8064=DIRECTION('',(-0.707106781186548,-0.707106781186547,0.));
#8065=DIRECTION('',(0.707106781186548,0.707106781186547,0.));
#8066=DIRECTION('center_axis',(-0.707106781186548,0.707106781186548,0.));
#8067=DIRECTION('ref_axis',(0.5,0.5,-0.707106781186547));
#8068=DIRECTION('',(0.707106781186548,-0.707106781186548,0.));
#8069=DIRECTION('',(-0.707106781186548,0.707106781186548,0.));
#8070=DIRECTION('center_axis',(0.923879532511286,-0.382683432365092,0.));
#8071=DIRECTION('ref_axis',(-0.382683432365091,-0.923879532511286,0.));
#8072=DIRECTION('center_axis',(-1.,0.,0.));
#8073=DIRECTION('ref_axis',(0.,0.707106781186548,-0.707106781186548));
#8074=DIRECTION('',(1.,0.,0.));
#8075=DIRECTION('',(-1.,0.,0.));
#8076=DIRECTION('center_axis',(0.923879532511286,0.382683432365092,0.));
#8077=DIRECTION('ref_axis',(0.382683432365092,-0.923879532511286,0.));
#8078=DIRECTION('center_axis',(0.707106781186548,0.707106781186548,0.));
#8079=DIRECTION('ref_axis',(0.5,-0.5,-0.707106781186547));
#8080=DIRECTION('',(0.707106781186548,0.707106781186548,0.));
#8081=DIRECTION('',(-0.707106781186548,-0.707106781186548,0.));
#8082=DIRECTION('center_axis',(-0.707106781186548,-0.707106781186548,0.));
#8083=DIRECTION('ref_axis',(-0.5,0.5,-0.707106781186547));
#8084=DIRECTION('',(0.707106781186548,0.707106781186548,0.));
#8085=DIRECTION('',(-0.707106781186548,-0.707106781186548,0.));
#8086=DIRECTION('center_axis',(0.382683432365092,0.923879532511286,0.));
#8087=DIRECTION('ref_axis',(0.923879532511286,-0.382683432365091,0.));
#8088=DIRECTION('center_axis',(0.,-1.,0.));
#8089=DIRECTION('ref_axis',(-0.707106781186548,0.,-0.707106781186548));
#8090=DIRECTION('',(0.,1.,0.));
#8091=DIRECTION('',(0.,-1.,0.));
#8092=DIRECTION('center_axis',(-0.382683432365092,0.923879532511286,0.));
#8093=DIRECTION('ref_axis',(0.923879532511286,0.382683432365092,0.));
#8094=DIRECTION('center_axis',(0.707106781186548,-0.707106781186548,0.));
#8095=DIRECTION('ref_axis',(-0.5,-0.5,-0.707106781186547));
#8096=DIRECTION('',(-0.707106781186548,0.707106781186548,0.));
#8097=DIRECTION('',(0.707106781186548,-0.707106781186548,0.));
#8098=DIRECTION('center_axis',(0.707106781186548,-0.707106781186548,0.));
#8099=DIRECTION('ref_axis',(0.,0.,-1.));
#8100=DIRECTION('',(0.,0.,1.));
#8101=DIRECTION('',(0.707106781186548,0.707106781186548,0.));
#8102=DIRECTION('',(0.,0.,-1.));
#8103=DIRECTION('center_axis',(1.,0.,0.));
#8104=DIRECTION('ref_axis',(0.,1.,0.));
#8105=DIRECTION('',(0.,0.,1.));
#8106=DIRECTION('',(0.,1.,0.));
#8107=DIRECTION('center_axis',(0.707106781186548,-0.707106781186548,0.));
#8108=DIRECTION('ref_axis',(0.707106781186548,0.707106781186548,0.));
#8109=DIRECTION('',(0.,0.,1.));
#8110=DIRECTION('',(0.707106781186548,0.707106781186548,0.));
#8111=DIRECTION('center_axis',(4.56509835347174E-16,-1.,0.));
#8112=DIRECTION('ref_axis',(1.,4.56509835347174E-16,0.));
#8113=DIRECTION('',(0.,0.,-1.));
#8114=DIRECTION('',(1.,4.56509835347174E-16,0.));
#8115=DIRECTION('center_axis',(0.707106781186547,-0.707106781186548,0.));
#8116=DIRECTION('ref_axis',(0.,0.,-1.));
#8117=DIRECTION('',(0.,0.,1.));
#8118=DIRECTION('',(0.707106781186548,0.707106781186547,0.));
#8119=DIRECTION('center_axis',(1.,0.,0.));
#8120=DIRECTION('ref_axis',(0.,1.,0.));
#8121=DIRECTION('',(0.,0.,1.));
#8122=DIRECTION('',(0.,1.,0.));
#8123=DIRECTION('center_axis',(0.,0.,1.));
#8124=DIRECTION('ref_axis',(1.,0.,0.));
#8125=DIRECTION('center_axis',(0.707106781186548,-0.707106781186548,0.));
#8126=DIRECTION('ref_axis',(-0.500000000000005,-0.500000000000005,0.707106781186541));
#8127=DIRECTION('',(-0.707106781186548,0.707106781186548,0.));
#8128=DIRECTION('center_axis',(0.382683432365092,-0.923879532511286,0.));
#8129=DIRECTION('ref_axis',(-0.923879532511286,-0.382683432365092,0.));
#8130=DIRECTION('',(0.707106781186548,-0.707106781186548,0.));
#8131=DIRECTION('center_axis',(0.923879532511286,-0.382683432365092,0.));
#8132=DIRECTION('ref_axis',(-0.382683432365092,-0.923879532511286,0.));
#8133=DIRECTION('center_axis',(0.,-1.,0.));
#8134=DIRECTION('ref_axis',(-0.707106781186554,0.,0.707106781186541));
#8135=DIRECTION('',(0.,1.,0.));
#8136=DIRECTION('center_axis',(-0.382683432365092,-0.923879532511286,0.));
#8137=DIRECTION('ref_axis',(-0.923879532511286,0.382683432365092,0.));
#8138=DIRECTION('',(0.,-1.,0.));
#8139=DIRECTION('center_axis',(-0.707106781186548,-0.707106781186548,0.));
#8140=DIRECTION('ref_axis',(-0.500000000000005,0.500000000000005,0.707106781186541));
#8141=DIRECTION('',(0.707106781186548,0.707106781186548,0.));
#8142=DIRECTION('center_axis',(-0.923879532511286,-0.382683432365092,0.));
#8143=DIRECTION('ref_axis',(-0.382683432365092,0.923879532511286,0.));
#8144=DIRECTION('',(-0.707106781186548,-0.707106781186548,0.));
#8145=DIRECTION('center_axis',(-1.,0.,0.));
#8146=DIRECTION('ref_axis',(0.,0.707106781186554,0.707106781186541));
#8147=DIRECTION('',(1.,0.,0.));
#8148=DIRECTION('center_axis',(-0.923879532511286,0.382683432365092,0.));
#8149=DIRECTION('ref_axis',(0.382683432365092,0.923879532511286,0.));
#8150=DIRECTION('',(-1.,0.,0.));
#8151=DIRECTION('center_axis',(-0.707106781186548,0.707106781186548,0.));
#8152=DIRECTION('ref_axis',(0.500000000000005,0.500000000000005,0.707106781186541));
#8153=DIRECTION('',(0.707106781186548,-0.707106781186548,0.));
#8154=DIRECTION('center_axis',(-0.382683432365092,0.923879532511286,0.));
#8155=DIRECTION('ref_axis',(0.923879532511286,0.382683432365092,0.));
#8156=DIRECTION('',(-0.707106781186548,0.707106781186548,0.));
#8157=DIRECTION('center_axis',(0.,1.,0.));
#8158=DIRECTION('ref_axis',(0.707106781186554,0.,0.707106781186541));
#8159=DIRECTION('',(0.,-1.,0.));
#8160=DIRECTION('center_axis',(0.382683432365093,0.923879532511285,0.));
#8161=DIRECTION('ref_axis',(0.923879532511285,-0.382683432365093,0.));
#8162=DIRECTION('center_axis',(-0.707106781186548,-0.707106781186547,0.));
#8163=DIRECTION('ref_axis',(0.5,-0.5,0.707106781186547));
#8164=DIRECTION('',(-0.707106781186548,-0.707106781186547,0.));
#8165=DIRECTION('center_axis',(0.923879532511287,0.38268343236509,0.));
#8166=DIRECTION('ref_axis',(-0.38268343236509,0.923879532511287,0.));
#8167=DIRECTION('center_axis',(1.,4.56509835347174E-16,0.));
#8168=DIRECTION('ref_axis',(0.,-0.707106781186557,0.707106781186538));
#8169=DIRECTION('',(-1.,-4.56509835347174E-16,0.));
#8170=DIRECTION('center_axis',(0.92387953251129,0.382683432365082,0.));
#8171=DIRECTION('ref_axis',(-0.382683432365082,0.92387953251129,0.));
#8172=DIRECTION('center_axis',(0.707106781186548,0.707106781186548,0.));
#8173=DIRECTION('ref_axis',(0.500000000000005,-0.500000000000005,0.707106781186541));
#8174=DIRECTION('',(-0.707106781186548,-0.707106781186548,0.));
#8175=DIRECTION('center_axis',(0.382683432365087,0.923879532511288,0.));
#8176=DIRECTION('ref_axis',(-0.923879532511288,0.382683432365087,0.));
#8177=DIRECTION('center_axis',(0.,1.,0.));
#8178=DIRECTION('ref_axis',(0.707106781186557,0.,0.707106781186538));
#8179=DIRECTION('',(0.,-1.,0.));
#8180=DIRECTION('center_axis',(0.382683432365097,0.923879532511284,-8.4972791550864E-16));
#8181=DIRECTION('ref_axis',(0.923879532511284,-0.382683432365097,-2.05142465794793E-15));
#8182=DIRECTION('center_axis',(-0.707106781186548,-0.707106781186548,0.));
#8183=DIRECTION('ref_axis',(0.5,-0.5,0.707106781186547));
#8184=DIRECTION('',(-0.707106781186548,-0.707106781186548,0.));
#8185=DIRECTION('center_axis',(0.923879532511283,0.382683432365099,0.));
#8186=DIRECTION('ref_axis',(-0.382683432365099,0.923879532511283,0.));
#8187=DIRECTION('center_axis',(1.,0.,0.));
#8188=DIRECTION('ref_axis',(0.,-0.707106781186554,0.707106781186541));
#8189=DIRECTION('',(1.,0.,0.));
#8190=DIRECTION('',(-1.,0.,0.));
#8191=DIRECTION('center_axis',(0.,-1.,0.));
#8192=DIRECTION('ref_axis',(1.,0.,0.));
#8193=DIRECTION('',(0.,0.,1.));
#8194=DIRECTION('center_axis',(-0.707106781186548,-0.707106781186548,0.));
#8195=DIRECTION('ref_axis',(0.707106781186548,-0.707106781186548,0.));
#8196=DIRECTION('',(0.,0.,1.));
#8197=DIRECTION('center_axis',(0.,0.,1.));
#8198=DIRECTION('ref_axis',(1.,0.,0.));
#8199=DIRECTION('center_axis',(-1.,0.,0.));
#8200=DIRECTION('ref_axis',(0.,-1.,0.));
#8201=DIRECTION('',(0.,0.,1.));
#8202=DIRECTION('center_axis',(-0.707106781186548,0.707106781186548,0.));
#8203=DIRECTION('ref_axis',(-0.707106781186548,-0.707106781186548,0.));
#8204=DIRECTION('',(0.,0.,1.));
#8205=DIRECTION('center_axis',(0.,1.,0.));
#8206=DIRECTION('ref_axis',(-1.,0.,0.));
#8207=DIRECTION('',(0.,0.,1.));
#8208=DIRECTION('center_axis',(0.707106781186548,0.707106781186548,0.));
#8209=DIRECTION('ref_axis',(-0.707106781186548,0.707106781186548,0.));
#8210=DIRECTION('axis',(0.,0.,1.));
#8211=DIRECTION('refdir',(1.,0.,0.));
#8212=DIRECTION('center_axis',(0.,1.,0.));
#8213=DIRECTION('ref_axis',(0.707106781186548,0.,-0.707106781186548));
#8214=DIRECTION('',(0.,-1.,0.));
#8215=DIRECTION('center_axis',(0.38268343236509,0.923879532511287,0.));
#8216=DIRECTION('ref_axis',(0.923879532511287,-0.38268343236509,0.));
#8217=DIRECTION('',(0.,1.,0.));
#8218=DIRECTION('center_axis',(-0.382683432365087,-0.923879532511288,0.));
#8219=DIRECTION('ref_axis',(0.923879532511288,-0.382683432365087,0.));
#8220=DIRECTION('center_axis',(1.,0.,0.));
#8221=DIRECTION('ref_axis',(0.,-0.707106781186548,-0.707106781186548));
#8222=DIRECTION('',(1.,0.,0.));
#8223=DIRECTION('center_axis',(-0.923879532511287,-0.38268343236509,0.));
#8224=DIRECTION('ref_axis',(-0.38268343236509,0.923879532511287,0.));
#8225=DIRECTION('',(-1.,0.,0.));
#8226=DIRECTION('center_axis',(0.923879532511288,0.382683432365087,-5.80230514691304E-15));
#8227=DIRECTION('ref_axis',(-0.382683432365087,0.923879532511288,-1.40080037787048E-14));
#8228=DIRECTION('center_axis',(0.707106781186548,0.707106781186548,0.));
#8229=DIRECTION('ref_axis',(0.499999999999998,-0.499999999999998,-0.70710678118655));
#8230=DIRECTION('',(0.707106781186548,0.707106781186548,0.));
#8231=DIRECTION('center_axis',(-0.382683432365095,-0.923879532511285,0.));
#8232=DIRECTION('ref_axis',(-0.923879532511285,0.382683432365095,0.));
#8233=DIRECTION('',(-0.707106781186548,-0.707106781186548,0.));
#8234=DIRECTION('center_axis',(0.,-1.,0.));
#8235=DIRECTION('ref_axis',(0.707106781186548,0.,-0.707106781186548));
#8236=DIRECTION('',(0.,1.,0.));
#8237=DIRECTION('center_axis',(0.382683432365099,-0.923879532511283,-8.20569863179165E-15));
#8238=DIRECTION('ref_axis',(0.923879532511283,0.382683432365098,-1.98103089256172E-14));
#8239=DIRECTION('',(0.,-1.,0.));
#8240=DIRECTION('center_axis',(-0.707106781186548,0.707106781186548,0.));
#8241=DIRECTION('ref_axis',(0.499999999999998,0.499999999999998,-0.70710678118655));
#8242=DIRECTION('',(-0.707106781186548,0.707106781186548,0.));
#8243=DIRECTION('center_axis',(0.923879532511286,-0.382683432365092,0.));
#8244=DIRECTION('ref_axis',(-0.382683432365092,-0.923879532511286,0.));
#8245=DIRECTION('',(0.707106781186548,-0.707106781186548,0.));
#8246=DIRECTION('center_axis',(1.,0.,0.));
#8247=DIRECTION('ref_axis',(0.,0.707106781186548,-0.707106781186548));
#8248=DIRECTION('',(-1.,0.,0.));
#8249=DIRECTION('center_axis',(0.923879532511286,0.382683432365092,0.));
#8250=DIRECTION('ref_axis',(-0.382683432365092,0.923879532511286,0.));
#8251=DIRECTION('',(1.,0.,0.));
#8252=DIRECTION('center_axis',(-0.707106781186548,-0.707106781186548,0.));
#8253=DIRECTION('ref_axis',(-0.499999999999998,0.499999999999998,-0.70710678118655));
#8254=DIRECTION('',(0.707106781186548,0.707106781186548,0.));
#8255=DIRECTION('',(-0.707106781186548,-0.707106781186548,0.));
#8256=DIRECTION('center_axis',(0.382683432365092,0.923879532511286,0.));
#8257=DIRECTION('ref_axis',(0.923879532511286,-0.382683432365092,0.));
#8258=DIRECTION('center_axis',(0.,1.,0.));
#8259=DIRECTION('ref_axis',(-0.707106781186548,0.,-0.707106781186548));
#8260=DIRECTION('',(0.,1.,0.));
#8261=DIRECTION('',(0.,-1.,0.));
#8262=DIRECTION('center_axis',(-0.382683432365092,0.923879532511286,0.));
#8263=DIRECTION('ref_axis',(-0.923879532511286,-0.382683432365092,0.));
#8264=DIRECTION('center_axis',(0.707106781186548,-0.707106781186548,0.));
#8265=DIRECTION('ref_axis',(-0.499999999999998,-0.499999999999998,-0.70710678118655));
#8266=DIRECTION('',(-0.707106781186548,0.707106781186548,0.));
#8267=DIRECTION('',(0.707106781186548,-0.707106781186548,0.));
#8268=DIRECTION('center_axis',(-0.923879532511286,0.382683432365092,0.));
#8269=DIRECTION('ref_axis',(0.382683432365092,0.923879532511286,0.));
#8270=DIRECTION('center_axis',(-1.,0.,0.));
#8271=DIRECTION('ref_axis',(0.,-0.707106781186548,-0.707106781186548));
#8272=DIRECTION('',(-1.,0.,0.));
#8273=DIRECTION('',(1.,0.,0.));
#8274=DIRECTION('center_axis',(-0.923879532511286,-0.382683432365092,4.10284931589584E-15));
#8275=DIRECTION('ref_axis',(0.382683432365092,-0.923879532511286,9.90515446280885E-15));
#8276=DIRECTION('center_axis',(0.707106781186548,0.707106781186548,0.));
#8277=DIRECTION('ref_axis',(0.499999999999998,-0.499999999999998,-0.70710678118655));
#8278=DIRECTION('',(-0.707106781186548,-0.707106781186548,0.));
#8279=DIRECTION('',(0.707106781186548,0.707106781186548,0.));
#8280=DIRECTION('center_axis',(0.707106781186548,0.707106781186548,0.));
#8281=DIRECTION('ref_axis',(0.499999999999998,-0.499999999999998,-0.70710678118655));
#8282=DIRECTION('',(-0.707106781186548,-0.707106781186548,0.));
#8283=DIRECTION('',(0.707106781186548,0.707106781186548,0.));
#8284=DIRECTION('center_axis',(-0.707106781186548,-0.707106781186548,0.));
#8285=DIRECTION('ref_axis',(0.,0.,1.));
#8286=DIRECTION('',(0.,0.,1.));
#8287=DIRECTION('',(0.707106781186548,-0.707106781186548,0.));
#8288=DIRECTION('',(0.,0.,-1.));
#8289=DIRECTION('center_axis',(0.,-1.,0.));
#8290=DIRECTION('ref_axis',(1.,0.,0.));
#8291=DIRECTION('',(0.,0.,-1.));
#8292=DIRECTION('',(1.,0.,0.));
#8293=DIRECTION('center_axis',(0.707106781186548,-0.707106781186548,0.));
#8294=DIRECTION('ref_axis',(0.,0.,-1.));
#8295=DIRECTION('',(0.,0.,1.));
#8296=DIRECTION('',(0.707106781186548,0.707106781186548,0.));
#8297=DIRECTION('center_axis',(1.,0.,0.));
#8298=DIRECTION('ref_axis',(0.,1.,0.));
#8299=DIRECTION('',(0.,0.,-1.));
#8300=DIRECTION('',(0.,1.,0.));
#8301=DIRECTION('center_axis',(0.707106781186548,-0.707106781186548,0.));
#8302=DIRECTION('ref_axis',(0.,0.,-1.));
#8303=DIRECTION('',(0.,0.,1.));
#8304=DIRECTION('',(0.707106781186548,0.707106781186548,0.));
#8305=DIRECTION('center_axis',(0.,-1.,0.));
#8306=DIRECTION('ref_axis',(1.,0.,0.));
#8307=DIRECTION('',(0.,0.,-1.));
#8308=DIRECTION('',(1.,0.,0.));
#8309=DIRECTION('center_axis',(0.,0.,1.));
#8310=DIRECTION('ref_axis',(-1.,0.,0.));
#8311=DIRECTION('center_axis',(0.,1.,0.));
#8312=DIRECTION('ref_axis',(0.707106781186551,0.,0.707106781186544));
#8313=DIRECTION('',(0.,-1.,0.));
#8314=DIRECTION('center_axis',(0.38268343236509,0.923879532511287,0.));
#8315=DIRECTION('ref_axis',(0.923879532511287,-0.38268343236509,0.));
#8316=DIRECTION('center_axis',(0.382683432365087,0.923879532511288,0.));
#8317=DIRECTION('ref_axis',(0.923879532511288,-0.382683432365087,0.));
#8318=DIRECTION('center_axis',(-0.707106781186548,-0.707106781186548,0.));
#8319=DIRECTION('ref_axis',(0.499999999999998,-0.499999999999998,0.70710678118655));
#8320=DIRECTION('',(-0.707106781186548,-0.707106781186548,0.));
#8321=DIRECTION('center_axis',(0.923879532511285,0.382683432365095,-4.10284931589581E-15));
#8322=DIRECTION('ref_axis',(-0.382683432365095,0.923879532511285,9.905154462809E-15));
#8323=DIRECTION('center_axis',(1.,0.,0.));
#8324=DIRECTION('ref_axis',(0.,-0.707106781186548,0.707106781186548));
#8325=DIRECTION('',(-1.,0.,0.));
#8326=DIRECTION('center_axis',(0.923879532511286,-0.382683432365092,0.));
#8327=DIRECTION('ref_axis',(-0.382683432365092,-0.923879532511286,0.));
#8328=DIRECTION('center_axis',(-0.707106781186548,0.707106781186548,0.));
#8329=DIRECTION('ref_axis',(-0.499999999999998,-0.499999999999998,0.70710678118655));
#8330=DIRECTION('',(-0.707106781186548,0.707106781186548,0.));
#8331=DIRECTION('center_axis',(0.382683432365092,-0.923879532511286,0.));
#8332=DIRECTION('ref_axis',(0.923879532511286,0.382683432365092,0.));
#8333=DIRECTION('center_axis',(0.,-1.,0.));
#8334=DIRECTION('ref_axis',(-0.707106781186548,0.,0.707106781186548));
#8335=DIRECTION('',(0.,1.,0.));
#8336=DIRECTION('center_axis',(-0.382683432365092,-0.923879532511286,0.));
#8337=DIRECTION('ref_axis',(-0.923879532511286,0.382683432365092,0.));
#8338=DIRECTION('',(0.,-1.,0.));
#8339=DIRECTION('center_axis',(0.707106781186548,0.707106781186548,0.));
#8340=DIRECTION('ref_axis',(-0.499999999999998,0.499999999999998,0.70710678118655));
#8341=DIRECTION('',(-0.707106781186548,-0.707106781186548,0.));
#8342=DIRECTION('',(0.707106781186548,0.707106781186548,0.));
#8343=DIRECTION('center_axis',(-0.923879532511286,-0.382683432365092,0.));
#8344=DIRECTION('ref_axis',(0.382683432365092,-0.923879532511286,0.));
#8345=DIRECTION('center_axis',(-1.,0.,0.));
#8346=DIRECTION('ref_axis',(0.,0.707106781186548,0.707106781186548));
#8347=DIRECTION('',(-1.,0.,0.));
#8348=DIRECTION('',(1.,0.,0.));
#8349=DIRECTION('center_axis',(-0.923879532511286,0.382683432365092,0.));
#8350=DIRECTION('ref_axis',(0.382683432365092,0.923879532511286,0.));
#8351=DIRECTION('center_axis',(0.707106781186548,-0.707106781186548,0.));
#8352=DIRECTION('ref_axis',(0.499999999999998,0.499999999999998,0.70710678118655));
#8353=DIRECTION('',(-0.707106781186548,0.707106781186548,0.));
#8354=DIRECTION('',(0.707106781186548,-0.707106781186548,0.));
#8355=DIRECTION('center_axis',(-0.382683432365092,0.923879532511286,0.));
#8356=DIRECTION('ref_axis',(-0.923879532511286,-0.382683432365092,0.));
#8357=DIRECTION('center_axis',(0.,1.,0.));
#8358=DIRECTION('ref_axis',(0.707106781186548,0.,0.707106781186548));
#8359=DIRECTION('',(0.,1.,0.));
#8360=DIRECTION('',(0.,-1.,0.));
#8361=DIRECTION('center_axis',(0.382683432365092,0.923879532511286,-4.10284931589584E-15));
#8362=DIRECTION('ref_axis',(0.923879532511286,-0.382683432365092,-9.90515446280885E-15));
#8363=DIRECTION('center_axis',(-0.707106781186548,-0.707106781186548,0.));
#8364=DIRECTION('ref_axis',(0.499999999999998,-0.499999999999998,0.70710678118655));
#8365=DIRECTION('',(0.707106781186548,0.707106781186548,0.));
#8366=DIRECTION('',(-0.707106781186548,-0.707106781186548,0.));
#8367=DIRECTION('center_axis',(0.923879532511287,0.38268343236509,0.));
#8368=DIRECTION('ref_axis',(-0.38268343236509,0.923879532511287,0.));
#8369=DIRECTION('center_axis',(1.,0.,0.));
#8370=DIRECTION('ref_axis',(0.,-0.707106781186551,0.707106781186544));
#8371=DIRECTION('',(-1.,0.,0.));
#8372=DIRECTION('center_axis',(0.923879532511288,0.382683432365087,5.80230514691306E-15));
#8373=DIRECTION('ref_axis',(-0.382683432365087,0.923879532511288,1.40080037787049E-14));
#8374=DIRECTION('center_axis',(-0.707106781186548,-0.707106781186548,0.));
#8375=DIRECTION('ref_axis',(0.499999999999998,-0.499999999999998,0.70710678118655));
#8376=DIRECTION('',(-0.707106781186548,-0.707106781186548,0.));
#8377=DIRECTION('center_axis',(0.707106781186548,0.707106781186548,0.));
#8378=DIRECTION('ref_axis',(0.,0.,-1.));
#8379=DIRECTION('',(0.,0.,1.));
#8380=DIRECTION('',(0.,0.,-1.));
#8381=DIRECTION('center_axis',(1.,0.,0.));
#8382=DIRECTION('ref_axis',(0.,1.,0.));
#8383=DIRECTION('',(0.,0.,1.));
#8384=DIRECTION('center_axis',(0.707106781186548,-0.707106781186548,0.));
#8385=DIRECTION('ref_axis',(0.,0.,-1.));
#8386=DIRECTION('center_axis',(0.,0.,1.));
#8387=DIRECTION('ref_axis',(1.,0.,0.));
#8388=DIRECTION('center_axis',(-0.707106781186548,0.707106781186548,0.));
#8389=DIRECTION('ref_axis',(0.,0.,1.));
#8390=DIRECTION('',(0.,0.,1.));
#8391=DIRECTION('',(0.,0.,-1.));
#8392=DIRECTION('center_axis',(0.,1.,0.));
#8393=DIRECTION('ref_axis',(-1.,0.,0.));
#8394=DIRECTION('center_axis',(-1.,0.,0.));
#8395=DIRECTION('ref_axis',(0.,-1.,0.));
#8396=DIRECTION('',(0.,0.,1.));
#8397=DIRECTION('',(1.,0.,0.));
#8398=DIRECTION('',(0.,0.,1.));
#8399=DIRECTION('',(1.,0.,0.));
#8400=DIRECTION('',(0.,0.,1.));
#8401=DIRECTION('',(1.,0.,0.));
#8402=DIRECTION('',(0.,0.,1.));
#8403=DIRECTION('',(1.,0.,0.));
#8404=DIRECTION('',(0.,0.,1.));
#8405=DIRECTION('',(1.,0.,0.));
#8406=DIRECTION('',(0.,0.,1.));
#8407=DIRECTION('',(1.,0.,0.));
#8408=DIRECTION('',(0.,0.,1.));
#8409=DIRECTION('',(1.,0.,0.));
#8410=DIRECTION('',(0.,0.,1.));
#8411=DIRECTION('',(1.,0.,0.));
#8412=DIRECTION('',(0.,0.,1.));
#8413=DIRECTION('',(1.,0.,0.));
#8414=DIRECTION('',(0.,0.,1.));
#8415=DIRECTION('',(1.,0.,0.));
#8416=CARTESIAN_POINT('',(0.,0.,0.));
#8417=CARTESIAN_POINT('',(0.,0.,0.));
#8418=CARTESIAN_POINT('Origin',(-65.371725664246,-65.371725664246,20.));
#8419=CARTESIAN_POINT('',(-65.371725664246,-75.371725664246,20.));
#8420=CARTESIAN_POINT('Origin',(-65.371725664246,-65.371725664246,20.));
#8421=CARTESIAN_POINT('',(-65.371725664246,-75.371725664246,0.));
#8422=CARTESIAN_POINT('',(-65.371725664246,-75.371725664246,20.));
#8423=CARTESIAN_POINT('Origin',(-65.371725664246,-65.371725664246,0.));
#8424=CARTESIAN_POINT('Origin',(-83.0493951939097,-83.0493951939097,20.));
#8425=CARTESIAN_POINT('',(-83.0493951939097,-93.0493951939097,20.));
#8426=CARTESIAN_POINT('Origin',(-83.0493951939097,-83.0493951939097,20.));
#8427=CARTESIAN_POINT('',(-83.0493951939097,-93.0493951939097,0.));
#8428=CARTESIAN_POINT('',(-83.0493951939097,-93.0493951939097,20.));
#8429=CARTESIAN_POINT('Origin',(-83.0493951939097,-83.0493951939097,0.));
#8430=CARTESIAN_POINT('Origin',(-65.371725664246,65.371725664246,20.));
#8431=CARTESIAN_POINT('',(-75.371725664246,65.371725664246,20.));
#8432=CARTESIAN_POINT('Origin',(-65.371725664246,65.371725664246,20.));
#8433=CARTESIAN_POINT('',(-75.371725664246,65.371725664246,0.));
#8434=CARTESIAN_POINT('',(-75.371725664246,65.371725664246,20.));
#8435=CARTESIAN_POINT('Origin',(-65.371725664246,65.371725664246,0.));
#8436=CARTESIAN_POINT('Origin',(-83.0493951939097,83.0493951939097,20.));
#8437=CARTESIAN_POINT('',(-93.0493951939097,83.0493951939097,20.));
#8438=CARTESIAN_POINT('Origin',(-83.0493951939097,83.0493951939097,20.));
#8439=CARTESIAN_POINT('',(-93.0493951939097,83.0493951939097,0.));
#8440=CARTESIAN_POINT('',(-93.0493951939097,83.0493951939097,20.));
#8441=CARTESIAN_POINT('Origin',(-83.0493951939097,83.0493951939097,0.));
#8442=CARTESIAN_POINT('Origin',(65.371725664246,65.371725664246,20.));
#8443=CARTESIAN_POINT('',(65.371725664246,75.371725664246,20.));
#8444=CARTESIAN_POINT('Origin',(65.371725664246,65.371725664246,20.));
#8445=CARTESIAN_POINT('',(65.371725664246,75.371725664246,0.));
#8446=CARTESIAN_POINT('',(65.371725664246,75.371725664246,20.));
#8447=CARTESIAN_POINT('Origin',(65.371725664246,65.371725664246,0.));
#8448=CARTESIAN_POINT('Origin',(83.0493951939097,83.0493951939097,20.));
#8449=CARTESIAN_POINT('',(83.0493951939097,93.0493951939097,20.));
#8450=CARTESIAN_POINT('Origin',(83.0493951939097,83.0493951939097,20.));
#8451=CARTESIAN_POINT('',(83.0493951939097,93.0493951939097,0.));
#8452=CARTESIAN_POINT('',(83.0493951939097,93.0493951939097,20.));
#8453=CARTESIAN_POINT('Origin',(83.0493951939097,83.0493951939097,0.));
#8454=CARTESIAN_POINT('Origin',(83.0493951939097,-83.0493951939097,20.));
#8455=CARTESIAN_POINT('',(93.0493951939097,-83.0493951939097,20.));
#8456=CARTESIAN_POINT('Origin',(83.0493951939097,-83.0493951939097,20.));
#8457=CARTESIAN_POINT('',(93.0493951939097,-83.0493951939097,0.));
#8458=CARTESIAN_POINT('',(93.0493951939097,-83.0493951939097,20.));
#8459=CARTESIAN_POINT('Origin',(83.0493951939097,-83.0493951939097,0.));
#8460=CARTESIAN_POINT('Origin',(65.371725664246,-65.371725664246,20.));
#8461=CARTESIAN_POINT('',(75.371725664246,-65.371725664246,20.));
#8462=CARTESIAN_POINT('Origin',(65.371725664246,-65.371725664246,20.));
#8463=CARTESIAN_POINT('',(75.371725664246,-65.371725664246,0.));
#8464=CARTESIAN_POINT('',(75.371725664246,-65.371725664246,20.));
#8465=CARTESIAN_POINT('Origin',(65.371725664246,-65.371725664246,0.));
#8466=CARTESIAN_POINT('Origin',(-90.,90.,0.));
#8467=CARTESIAN_POINT('',(-100.,90.,20.));
#8468=CARTESIAN_POINT('',(-90.,100.,20.));
#8469=CARTESIAN_POINT('Origin',(-90.,90.,20.));
#8470=CARTESIAN_POINT('',(-90.,100.,0.));
#8471=CARTESIAN_POINT('',(-90.,100.,0.));
#8472=CARTESIAN_POINT('',(-100.,90.,0.));
#8473=CARTESIAN_POINT('Origin',(-90.,90.,0.));
#8474=CARTESIAN_POINT('',(-100.,90.,0.));
#8475=CARTESIAN_POINT('Origin',(-100.,100.,0.));
#8476=CARTESIAN_POINT('',(-100.,-90.,0.));
#8477=CARTESIAN_POINT('',(-100.,-100.,0.));
#8478=CARTESIAN_POINT('',(-100.,-90.,20.));
#8479=CARTESIAN_POINT('',(-100.,-90.,0.));
#8480=CARTESIAN_POINT('',(-100.,-100.,20.));
#8481=CARTESIAN_POINT('Origin',(0.,0.,0.));
#8482=CARTESIAN_POINT('',(90.,100.,0.));
#8483=CARTESIAN_POINT('',(-100.,100.,0.));
#8484=CARTESIAN_POINT('',(100.,90.,0.));
#8485=CARTESIAN_POINT('Origin',(90.,90.,0.));
#8486=CARTESIAN_POINT('',(100.,-90.,0.));
#8487=CARTESIAN_POINT('',(100.,100.,0.));
#8488=CARTESIAN_POINT('',(90.,-100.,0.));
#8489=CARTESIAN_POINT('Origin',(90.,-90.,0.));
#8490=CARTESIAN_POINT('',(-90.,-100.,0.));
#8491=CARTESIAN_POINT('',(100.,-100.,0.));
#8492=CARTESIAN_POINT('Origin',(-90.,-90.,0.));
#8493=CARTESIAN_POINT('Origin',(90.,90.,0.));
#8494=CARTESIAN_POINT('',(90.,100.,20.));
#8495=CARTESIAN_POINT('',(100.,90.,20.));
#8496=CARTESIAN_POINT('Origin',(90.,90.,20.));
#8497=CARTESIAN_POINT('',(100.,90.,0.));
#8498=CARTESIAN_POINT('',(90.,100.,0.));
#8499=CARTESIAN_POINT('Origin',(100.,-100.,0.));
#8500=CARTESIAN_POINT('',(100.,-90.,20.));
#8501=CARTESIAN_POINT('',(100.,100.,20.));
#8502=CARTESIAN_POINT('',(100.,-90.,0.));
#8503=CARTESIAN_POINT('Origin',(90.,-90.,0.));
#8504=CARTESIAN_POINT('',(90.,-100.,20.));
#8505=CARTESIAN_POINT('Origin',(90.,-90.,20.));
#8506=CARTESIAN_POINT('',(90.,-100.,0.));
#8507=CARTESIAN_POINT('Origin',(-90.,-90.,0.));
#8508=CARTESIAN_POINT('',(-90.,-100.,20.));
#8509=CARTESIAN_POINT('Origin',(-90.,-90.,20.));
#8510=CARTESIAN_POINT('',(-90.,-100.,0.));
#8511=CARTESIAN_POINT('Origin',(-100.,-100.,0.));
#8512=CARTESIAN_POINT('',(100.,-100.,20.));
#8513=CARTESIAN_POINT('Origin',(100.,100.,0.));
#8514=CARTESIAN_POINT('',(-100.,100.,20.));
#8515=CARTESIAN_POINT('Origin',(0.,0.,20.));
#8516=CARTESIAN_POINT('',(0.,0.,0.));
#8517=CARTESIAN_POINT('Origin',(61.,-6.90286596077709,56.9950844505733));
#8518=CARTESIAN_POINT('',(61.,-9.90286596077709,56.9950844505733));
#8519=CARTESIAN_POINT('Origin',(61.,-6.90286596077709,56.9950844505733));
#8520=CARTESIAN_POINT('',(50.,-9.90286596077709,56.9950844505733));
#8521=CARTESIAN_POINT('',(61.,-9.90286596077709,56.9950844505733));
#8522=CARTESIAN_POINT('Origin',(50.,-6.90286596077709,56.9950844505733));
#8523=CARTESIAN_POINT('Origin',(60.5,18.8741278186466,61.5));
#8524=CARTESIAN_POINT('',(61.,6.45991425627347,61.));
#8525=CARTESIAN_POINT('',(61.,28.4599142562735,61.));
#8526=CARTESIAN_POINT('',(61.,18.8741278186466,61.));
#8527=CARTESIAN_POINT('',(60.,28.8741278186466,62.));
#8528=CARTESIAN_POINT('',(61.,28.4599142562735,61.));
#8529=CARTESIAN_POINT('',(60.,6.87412781864656,62.));
#8530=CARTESIAN_POINT('',(60.,18.8741278186466,62.));
#8531=CARTESIAN_POINT('',(61.,6.45991425627347,61.));
#8532=CARTESIAN_POINT('Origin',(60.5,24.5205744280533,65.6464466094067));
#8533=CARTESIAN_POINT('',(61.,28.8741278186466,60.5857864376269));
#8534=CARTESIAN_POINT('',(61.,24.16702103746,65.2928932188134));
#8535=CARTESIAN_POINT('',(60.,29.8741278186466,61.));
#8536=CARTESIAN_POINT('',(61.,28.8741278186466,60.5857864376269));
#8537=CARTESIAN_POINT('',(60.,24.8741278186466,66.));
#8538=CARTESIAN_POINT('Origin',(60.5,29.3741278186466,54.));
#8539=CARTESIAN_POINT('',(61.,28.8741278186466,51.4142135623731));
#8540=CARTESIAN_POINT('',(61.,28.8741278186466,54.));
#8541=CARTESIAN_POINT('',(60.,29.8741278186466,51.));
#8542=CARTESIAN_POINT('',(61.,28.8741278186466,51.4142135623731));
#8543=CARTESIAN_POINT('',(60.,29.8741278186466,54.));
#8544=CARTESIAN_POINT('Origin',(60.5,25.5205744280533,47.3535533905933));
#8545=CARTESIAN_POINT('',(61.,28.4599142562735,51.));
#8546=CARTESIAN_POINT('',(61.,25.16702103746,47.7071067811865));
#8547=CARTESIAN_POINT('',(60.,28.8741278186466,50.));
#8548=CARTESIAN_POINT('',(61.,28.4599142562735,51.));
#8549=CARTESIAN_POINT('',(60.,25.8741278186466,47.));
#8550=CARTESIAN_POINT('Origin',(60.5,-3.12587218135344,50.5));
#8551=CARTESIAN_POINT('',(61.,-12.7116586189803,51.));
#8552=CARTESIAN_POINT('',(61.,-3.12587218135344,51.));
#8553=CARTESIAN_POINT('',(60.,-13.1258721813534,50.));
#8554=CARTESIAN_POINT('',(61.,-12.7116586189803,51.));
#8555=CARTESIAN_POINT('',(60.,-3.12587218135344,50.));
#8556=CARTESIAN_POINT('Origin',(60.5,-9.77231879076014,47.3535533905933));
#8557=CARTESIAN_POINT('',(60.,-14.1258721813534,51.));
#8558=CARTESIAN_POINT('',(60.,-10.1258721813534,47.));
#8559=CARTESIAN_POINT('',(61.,-13.1258721813534,51.4142135623731));
#8560=CARTESIAN_POINT('',(61.,-9.41876540016687,47.7071067811865));
#8561=CARTESIAN_POINT('',(61.,-13.1258721813534,51.4142135623731));
#8562=CARTESIAN_POINT('Origin',(60.5,-13.6258721813534,62.));
#8563=CARTESIAN_POINT('',(60.,-14.1258721813534,65.));
#8564=CARTESIAN_POINT('',(60.,-14.1258721813534,62.));
#8565=CARTESIAN_POINT('',(61.,-13.1258721813534,64.5857864376269));
#8566=CARTESIAN_POINT('',(61.,-13.1258721813534,62.));
#8567=CARTESIAN_POINT('',(61.,-13.1258721813534,64.5857864376269));
#8568=CARTESIAN_POINT('Origin',(60.5,-9.77231879076014,68.6464466094067));
#8569=CARTESIAN_POINT('',(60.,-13.1258721813534,66.));
#8570=CARTESIAN_POINT('',(60.,-10.1258721813534,69.));
#8571=CARTESIAN_POINT('',(61.,-12.7116586189803,65.));
#8572=CARTESIAN_POINT('',(61.,-9.41876540016687,68.2928932188135));
#8573=CARTESIAN_POINT('',(61.,-12.7116586189803,65.));
#8574=CARTESIAN_POINT('Origin',(60.5,6.87412781864656,65.5));
#8575=CARTESIAN_POINT('',(60.,4.87412781864656,66.));
#8576=CARTESIAN_POINT('',(60.,6.87412781864656,66.));
#8577=CARTESIAN_POINT('',(61.,4.45991425627347,65.));
#8578=CARTESIAN_POINT('',(61.,6.87412781864656,65.));
#8579=CARTESIAN_POINT('',(61.,4.45991425627347,65.));
#8580=CARTESIAN_POINT('Origin',(60.5,7.52057442805329,62.6464466094067));
#8581=CARTESIAN_POINT('',(60.,5.87412781864656,65.));
#8582=CARTESIAN_POINT('',(60.,7.87412781864656,63.));
#8583=CARTESIAN_POINT('',(61.,4.87412781864656,64.5857864376269));
#8584=CARTESIAN_POINT('',(61.,7.16702103746002,62.2928932188135));
#8585=CARTESIAN_POINT('',(61.,4.87412781864656,64.5857864376269));
#8586=CARTESIAN_POINT('Origin',(60.5,5.37412781864656,60.));
#8587=CARTESIAN_POINT('',(60.,5.87412781864656,63.));
#8588=CARTESIAN_POINT('',(60.,5.87412781864656,60.));
#8589=CARTESIAN_POINT('',(61.,4.87412781864656,62.5857864376269));
#8590=CARTESIAN_POINT('',(61.,4.87412781864656,60.));
#8591=CARTESIAN_POINT('',(61.,4.87412781864656,62.5857864376269));
#8592=CARTESIAN_POINT('Origin',(60.5,7.52057442805329,60.6464466094067));
#8593=CARTESIAN_POINT('',(60.,7.87412781864656,61.));
#8594=CARTESIAN_POINT('',(61.,7.16702103746002,60.2928932188135));
#8595=CARTESIAN_POINT('Origin',(50.,-13.6258721813534,65.5));
#8596=CARTESIAN_POINT('',(50.,-13.1258721813534,66.));
#8597=CARTESIAN_POINT('',(50.,-13.1258721813534,66.));
#8598=CARTESIAN_POINT('',(50.,-14.1258721813534,65.));
#8599=CARTESIAN_POINT('',(50.,-10.1258721813534,69.));
#8600=CARTESIAN_POINT('',(50.,-14.1258721813534,65.));
#8601=CARTESIAN_POINT('Origin',(50.,5.87412781864656,66.));
#8602=CARTESIAN_POINT('',(50.,4.87412781864656,66.));
#8603=CARTESIAN_POINT('',(50.,4.87412781864656,66.));
#8604=CARTESIAN_POINT('',(50.,5.87412781864656,66.));
#8605=CARTESIAN_POINT('Origin',(50.,5.37412781864656,65.5));
#8606=CARTESIAN_POINT('',(50.,5.87412781864656,65.));
#8607=CARTESIAN_POINT('',(50.,5.87412781864656,65.));
#8608=CARTESIAN_POINT('',(50.,7.87412781864656,63.));
#8609=CARTESIAN_POINT('Origin',(50.,5.87412781864656,62.));
#8610=CARTESIAN_POINT('',(50.,5.87412781864656,63.));
#8611=CARTESIAN_POINT('',(50.,5.87412781864656,63.));
#8612=CARTESIAN_POINT('',(50.,5.87412781864656,50.));
#8613=CARTESIAN_POINT('Origin',(50.,6.37412781864656,62.5));
#8614=CARTESIAN_POINT('',(50.,6.87412781864656,62.));
#8615=CARTESIAN_POINT('',(50.,6.87412781864656,62.));
#8616=CARTESIAN_POINT('',(50.,7.87412781864656,61.));
#8617=CARTESIAN_POINT('Origin',(50.,29.8741278186466,62.));
#8618=CARTESIAN_POINT('',(50.,28.8741278186466,62.));
#8619=CARTESIAN_POINT('',(50.,28.8741278186466,62.));
#8620=CARTESIAN_POINT('',(50.,29.8741278186466,62.));
#8621=CARTESIAN_POINT('Origin',(61.,7.87412781864656,58.));
#8622=CARTESIAN_POINT('Origin',(50.,-13.6258721813534,50.5));
#8623=CARTESIAN_POINT('',(50.,-14.1258721813534,51.));
#8624=CARTESIAN_POINT('',(50.,-14.1258721813534,51.));
#8625=CARTESIAN_POINT('',(50.,-13.1258721813534,50.));
#8626=CARTESIAN_POINT('',(50.,-10.1258721813534,47.));
#8627=CARTESIAN_POINT('',(50.,-13.1258721813534,50.));
#8628=CARTESIAN_POINT('Origin',(50.,-14.1258721813534,50.));
#8629=CARTESIAN_POINT('',(50.,28.8741278186466,50.));
#8630=CARTESIAN_POINT('',(50.,-14.1258721813534,50.));
#8631=CARTESIAN_POINT('',(50.,28.8741278186466,50.));
#8632=CARTESIAN_POINT('Origin',(50.,7.87412781864656,58.));
#8633=CARTESIAN_POINT('',(50.,-14.1258721813534,66.));
#8634=CARTESIAN_POINT('',(50.,29.8741278186466,61.));
#8635=CARTESIAN_POINT('',(50.,24.8741278186466,66.));
#8636=CARTESIAN_POINT('',(50.,29.8741278186466,51.));
#8637=CARTESIAN_POINT('',(50.,29.8741278186466,50.));
#8638=CARTESIAN_POINT('',(50.,25.8741278186466,47.));
#8639=CARTESIAN_POINT('Origin',(50.,29.3741278186466,50.5));
#8640=CARTESIAN_POINT('',(50.,29.8741278186466,51.));
#8641=CARTESIAN_POINT('Origin',(50.,29.8741278186466,50.));
#8642=CARTESIAN_POINT('',(50.,29.8741278186466,61.));
#8643=CARTESIAN_POINT('Origin',(50.,29.3741278186466,61.5));
#8644=CARTESIAN_POINT('Origin',(50.,-14.1258721813534,66.));
#8645=CARTESIAN_POINT('',(0.,0.,0.));
#8646=CARTESIAN_POINT('Origin',(-8.5,-49.,85.));
#8647=CARTESIAN_POINT('',(-4.5,-49.,90.));
#8648=CARTESIAN_POINT('',(-8.5,-49.,86.));
#8649=CARTESIAN_POINT('Origin',(-8.5,-49.,90.));
#8650=CARTESIAN_POINT('',(-8.5,-50.,85.));
#8651=CARTESIAN_POINT('Origin',(-8.5,-49.,85.));
#8652=CARTESIAN_POINT('',(-4.5,-50.,89.8989794855664));
#8653=CARTESIAN_POINT('Ctrl Pts',(-8.5,-50.,85.));
#8654=CARTESIAN_POINT('Ctrl Pts',(-7.96337444213282,-50.,85.2683127789336));
#8655=CARTESIAN_POINT('Ctrl Pts',(-7.37146954918018,-50.,85.5644396994907));
#8656=CARTESIAN_POINT('Ctrl Pts',(-6.29356794340685,-50.,86.2912190109971));
#8657=CARTESIAN_POINT('Ctrl Pts',(-5.81057468241034,-50.,86.7263159860593));
#8658=CARTESIAN_POINT('Ctrl Pts',(-5.16020070925815,-50.,87.5716441011679));
#8659=CARTESIAN_POINT('Ctrl Pts',(-4.89013404243441,-50.,88.0621303350776));
#8660=CARTESIAN_POINT('Ctrl Pts',(-4.59098232128521,-50.,88.9247155210796));
#8661=CARTESIAN_POINT('Ctrl Pts',(-4.5,-50.,89.4525943977152));
#8662=CARTESIAN_POINT('Ctrl Pts',(-4.5,-50.,89.8989794855664));
#8663=CARTESIAN_POINT('Origin',(-4.5,-49.,85.));
#8664=CARTESIAN_POINT('Origin',(-8.5,0.,90.));
#8665=CARTESIAN_POINT('',(-4.5,49.,90.));
#8666=CARTESIAN_POINT('',(-8.5,49.,86.));
#8667=CARTESIAN_POINT('Origin',(-8.5,49.,90.));
#8668=CARTESIAN_POINT('',(-8.5,0.,86.));
#8669=CARTESIAN_POINT('',(-4.5,0.,90.));
#8670=CARTESIAN_POINT('Origin',(-8.5,49.,85.));
#8671=CARTESIAN_POINT('',(-4.5,50.,89.8989794855664));
#8672=CARTESIAN_POINT('',(-8.5,50.,85.));
#8673=CARTESIAN_POINT('Ctrl Pts',(-4.5,50.,89.8989794855664));
#8674=CARTESIAN_POINT('Ctrl Pts',(-4.5,50.,89.4525943977152));
#8675=CARTESIAN_POINT('Ctrl Pts',(-4.59098232128521,50.,88.9247155210796));
#8676=CARTESIAN_POINT('Ctrl Pts',(-4.89013404243441,50.,88.0621303350776));
#8677=CARTESIAN_POINT('Ctrl Pts',(-5.16020070925815,50.,87.5716441011679));
#8678=CARTESIAN_POINT('Ctrl Pts',(-5.81057468241034,50.,86.7263159860593));
#8679=CARTESIAN_POINT('Ctrl Pts',(-6.29356794340685,50.,86.2912190109971));
#8680=CARTESIAN_POINT('Ctrl Pts',(-7.37146954918018,50.,85.5644396994907));
#8681=CARTESIAN_POINT('Ctrl Pts',(-7.96337444213282,50.,85.2683127789336));
#8682=CARTESIAN_POINT('Ctrl Pts',(-8.5,50.,85.));
#8683=CARTESIAN_POINT('Origin',(-8.5,49.,85.));
#8684=CARTESIAN_POINT('Origin',(-4.5,49.,85.));
#8685=CARTESIAN_POINT('Origin',(-4.5,0.,102.763485025341));
#8686=CARTESIAN_POINT('',(-4.5,-50.,120.526970050681));
#8687=CARTESIAN_POINT('',(-4.5,-50.,85.));
#8688=CARTESIAN_POINT('',(-4.5,50.,93.7320508075689));
#8689=CARTESIAN_POINT('',(-4.5,46.0011587545003,94.8035370899608));
#8690=CARTESIAN_POINT('',(-4.5,50.,85.));
#8691=CARTESIAN_POINT('Origin',(9.5,49.,85.));
#8692=CARTESIAN_POINT('',(5.5,49.,90.));
#8693=CARTESIAN_POINT('',(9.5,49.,86.));
#8694=CARTESIAN_POINT('Origin',(9.5,49.,90.));
#8695=CARTESIAN_POINT('',(9.5,50.,85.));
#8696=CARTESIAN_POINT('Origin',(9.5,49.,85.));
#8697=CARTESIAN_POINT('',(5.5,50.,89.8989794855664));
#8698=CARTESIAN_POINT('Ctrl Pts',(9.5,50.,85.));
#8699=CARTESIAN_POINT('Ctrl Pts',(8.96337444213282,50.,85.2683127789336));
#8700=CARTESIAN_POINT('Ctrl Pts',(8.37146954918018,50.,85.5644396994907));
#8701=CARTESIAN_POINT('Ctrl Pts',(7.29356794340685,50.,86.2912190109971));
#8702=CARTESIAN_POINT('Ctrl Pts',(6.81057468241033,50.,86.7263159860593));
#8703=CARTESIAN_POINT('Ctrl Pts',(6.16020070925815,50.,87.5716441011679));
#8704=CARTESIAN_POINT('Ctrl Pts',(5.8901340424344,50.,88.0621303350776));
#8705=CARTESIAN_POINT('Ctrl Pts',(5.59098232128521,50.,88.9247155210796));
#8706=CARTESIAN_POINT('Ctrl Pts',(5.5,50.,89.4525943977152));
#8707=CARTESIAN_POINT('Ctrl Pts',(5.5,50.,89.8989794855664));
#8708=CARTESIAN_POINT('Origin',(5.5,49.,85.));
#8709=CARTESIAN_POINT('Origin',(9.5,0.,90.));
#8710=CARTESIAN_POINT('',(5.5,-49.,90.));
#8711=CARTESIAN_POINT('',(9.5,-49.,86.));
#8712=CARTESIAN_POINT('Origin',(9.5,-49.,90.));
#8713=CARTESIAN_POINT('',(9.5,0.,86.));
#8714=CARTESIAN_POINT('',(5.5,0.,90.));
#8715=CARTESIAN_POINT('Origin',(9.5,-49.,85.));
#8716=CARTESIAN_POINT('',(5.5,-50.,89.8989794855664));
#8717=CARTESIAN_POINT('',(9.5,-50.,85.));
#8718=CARTESIAN_POINT('Ctrl Pts',(5.5,-50.,89.8989794855664));
#8719=CARTESIAN_POINT('Ctrl Pts',(5.5,-50.,89.4525943977152));
#8720=CARTESIAN_POINT('Ctrl Pts',(5.59098232128521,-50.,88.9247155210796));
#8721=CARTESIAN_POINT('Ctrl Pts',(5.8901340424344,-50.,88.0621303350776));
#8722=CARTESIAN_POINT('Ctrl Pts',(6.16020070925815,-50.,87.5716441011679));
#8723=CARTESIAN_POINT('Ctrl Pts',(6.81057468241033,-50.,86.7263159860593));
#8724=CARTESIAN_POINT('Ctrl Pts',(7.29356794340685,-50.,86.2912190109971));
#8725=CARTESIAN_POINT('Ctrl Pts',(8.37146954918018,-50.,85.5644396994907));
#8726=CARTESIAN_POINT('Ctrl Pts',(8.96337444213282,-50.,85.2683127789336));
#8727=CARTESIAN_POINT('Ctrl Pts',(9.5,-50.,85.));
#8728=CARTESIAN_POINT('Origin',(9.5,-49.,85.));
#8729=CARTESIAN_POINT('Origin',(5.5,-49.,85.));
#8730=CARTESIAN_POINT('Origin',(5.5,0.,102.763485025341));
#8731=CARTESIAN_POINT('',(5.5,50.,93.7320508075689));
#8732=CARTESIAN_POINT('',(5.5,50.,85.));
#8733=CARTESIAN_POINT('',(5.5,-50.,120.526970050681));
#8734=CARTESIAN_POINT('',(5.5,46.0011587545003,94.8035370899608));
#8735=CARTESIAN_POINT('',(5.5,-50.,85.));
#8736=CARTESIAN_POINT('Origin',(-32.4855257306532,-32.7240321735238,86.));
#8737=CARTESIAN_POINT('',(-29.4855257306532,-32.7240321735238,86.));
#8738=CARTESIAN_POINT('Origin',(-32.4855257306532,-32.7240321735238,86.));
#8739=CARTESIAN_POINT('',(-29.4855257306532,-32.7240321735238,74.));
#8740=CARTESIAN_POINT('',(-29.4855257306532,-32.7240321735238,86.));
#8741=CARTESIAN_POINT('Origin',(-32.4855257306532,-32.7240321735238,74.));
#8742=CARTESIAN_POINT('Origin',(32.5144742693468,32.2759678264762,86.));
#8743=CARTESIAN_POINT('',(35.5144742693468,32.2759678264762,86.));
#8744=CARTESIAN_POINT('Origin',(32.5144742693468,32.2759678264762,86.));
#8745=CARTESIAN_POINT('',(35.5144742693468,32.2759678264762,74.));
#8746=CARTESIAN_POINT('',(35.5144742693468,32.2759678264762,86.));
#8747=CARTESIAN_POINT('Origin',(32.5144742693468,32.2759678264762,74.));
#8748=CARTESIAN_POINT('Origin',(-32.4855257306532,32.2759678264762,86.));
#8749=CARTESIAN_POINT('',(-29.4855257306532,32.2759678264762,86.));
#8750=CARTESIAN_POINT('Origin',(-32.4855257306532,32.2759678264762,86.));
#8751=CARTESIAN_POINT('',(-29.4855257306532,32.2759678264762,74.));
#8752=CARTESIAN_POINT('',(-29.4855257306532,32.2759678264762,86.));
#8753=CARTESIAN_POINT('Origin',(-32.4855257306532,32.2759678264762,74.));
#8754=CARTESIAN_POINT('Origin',(32.5144742693468,-7.72403217352376,86.));
#8755=CARTESIAN_POINT('',(35.5144742693468,-7.72403217352376,86.));
#8756=CARTESIAN_POINT('Origin',(32.5144742693468,-7.72403217352376,86.));
#8757=CARTESIAN_POINT('',(35.5144742693468,-7.72403217352376,74.));
#8758=CARTESIAN_POINT('',(35.5144742693468,-7.72403217352376,86.));
#8759=CARTESIAN_POINT('Origin',(32.5144742693468,-7.72403217352376,74.));
#8760=CARTESIAN_POINT('Origin',(0.499999999999998,50.,93.7320508075689));
#8761=CARTESIAN_POINT('',(0.499999999999998,-50.,120.526970050681));
#8762=CARTESIAN_POINT('',(0.499999999999998,50.,93.7320508075689));
#8763=CARTESIAN_POINT('Origin',(22.5,49.,85.));
#8764=CARTESIAN_POINT('',(-45.,50.,85.));
#8765=CARTESIAN_POINT('',(22.5,50.,85.));
#8766=CARTESIAN_POINT('',(-44.5857864376269,49.,86.));
#8767=CARTESIAN_POINT('Origin',(-44.5857864376269,49.,85.));
#8768=CARTESIAN_POINT('',(22.5,49.,86.));
#8769=CARTESIAN_POINT('Origin',(22.5,49.,85.));
#8770=CARTESIAN_POINT('',(44.5857864376269,49.,86.));
#8771=CARTESIAN_POINT('',(22.5,49.,86.));
#8772=CARTESIAN_POINT('',(45.,50.,85.));
#8773=CARTESIAN_POINT('Origin',(44.5857864376269,49.,85.));
#8774=CARTESIAN_POINT('',(22.5,50.,85.));
#8775=CARTESIAN_POINT('Origin',(0.,0.,86.));
#8776=CARTESIAN_POINT('',(-49.,44.5857864376269,86.));
#8777=CARTESIAN_POINT('',(-45.5428932188135,48.0428932188135,86.));
#8778=CARTESIAN_POINT('',(-49.,-44.5857864376269,86.));
#8779=CARTESIAN_POINT('',(-49.,22.5,86.));
#8780=CARTESIAN_POINT('',(-44.5857864376269,-49.,86.));
#8781=CARTESIAN_POINT('',(-48.0428932188135,-45.5428932188135,86.));
#8782=CARTESIAN_POINT('',(-22.5,-49.,86.));
#8783=CARTESIAN_POINT('Origin',(0.,0.,86.));
#8784=CARTESIAN_POINT('',(15.5857864376269,-49.,86.));
#8785=CARTESIAN_POINT('',(-22.5,-49.,86.));
#8786=CARTESIAN_POINT('',(20.,-44.5857864376269,86.));
#8787=CARTESIAN_POINT('',(25.0428932188134,-39.5428932188134,86.));
#8788=CARTESIAN_POINT('',(20.,-30.8578643762691,86.));
#8789=CARTESIAN_POINT('',(20.,-25.,86.));
#8790=CARTESIAN_POINT('',(30.857864376269,-20.,86.));
#8791=CARTESIAN_POINT('',(22.860912703474,-27.9969516727951,86.));
#8792=CARTESIAN_POINT('',(44.5857864376269,-20.,86.));
#8793=CARTESIAN_POINT('',(15.6360389693211,-20.,86.));
#8794=CARTESIAN_POINT('',(49.,-15.5857864376269,86.));
#8795=CARTESIAN_POINT('',(39.5428932188134,-25.0428932188135,86.));
#8796=CARTESIAN_POINT('',(49.,44.5857864376269,86.));
#8797=CARTESIAN_POINT('',(49.,-10.5,86.));
#8798=CARTESIAN_POINT('',(48.0428932188135,45.5428932188135,86.));
#8799=CARTESIAN_POINT('Origin',(-22.5,-49.,85.));
#8800=CARTESIAN_POINT('',(-45.,-50.,85.));
#8801=CARTESIAN_POINT('Origin',(-44.5857864376269,-49.,85.));
#8802=CARTESIAN_POINT('',(-22.5,-50.,85.));
#8803=CARTESIAN_POINT('Origin',(-22.5,-49.,85.));
#8804=CARTESIAN_POINT('',(16.,-50.,85.));
#8805=CARTESIAN_POINT('',(-22.5,-50.,85.));
#8806=CARTESIAN_POINT('Origin',(15.5857864376269,-49.,85.));
#8807=CARTESIAN_POINT('Origin',(-22.5,-49.,75.));
#8808=CARTESIAN_POINT('',(-44.5857864376269,-49.,74.));
#8809=CARTESIAN_POINT('',(15.5857864376269,-49.,74.));
#8810=CARTESIAN_POINT('',(-22.5,-49.,74.));
#8811=CARTESIAN_POINT('',(16.,-50.,75.));
#8812=CARTESIAN_POINT('Origin',(15.5857864376269,-49.,75.));
#8813=CARTESIAN_POINT('',(-45.,-50.,75.));
#8814=CARTESIAN_POINT('',(-22.5,-50.,75.));
#8815=CARTESIAN_POINT('Origin',(-44.5857864376269,-49.,75.));
#8816=CARTESIAN_POINT('Origin',(20.,-25.,75.));
#8817=CARTESIAN_POINT('',(20.,-44.5857864376269,74.));
#8818=CARTESIAN_POINT('',(20.,-30.8578643762691,74.));
#8819=CARTESIAN_POINT('',(20.,-25.,74.));
#8820=CARTESIAN_POINT('',(21.,-31.2720779386421,75.));
#8821=CARTESIAN_POINT('Origin',(20.,-30.8578643762691,75.));
#8822=CARTESIAN_POINT('',(21.,-45.,75.));
#8823=CARTESIAN_POINT('',(21.,-25.,75.));
#8824=CARTESIAN_POINT('Origin',(20.,-44.5857864376269,75.));
#8825=CARTESIAN_POINT('Origin',(22.860912703474,-27.9969516727951,75.));
#8826=CARTESIAN_POINT('',(30.857864376269,-20.,74.));
#8827=CARTESIAN_POINT('',(22.860912703474,-27.9969516727951,74.));
#8828=CARTESIAN_POINT('',(31.2720779386421,-21.,75.));
#8829=CARTESIAN_POINT('Origin',(30.857864376269,-20.,75.));
#8830=CARTESIAN_POINT('',(23.5680194846605,-28.7040584539816,75.));
#8831=CARTESIAN_POINT('Origin',(49.,-10.5,75.));
#8832=CARTESIAN_POINT('',(50.,45.,75.));
#8833=CARTESIAN_POINT('',(50.,-16.,75.));
#8834=CARTESIAN_POINT('',(50.,-10.5,75.));
#8835=CARTESIAN_POINT('',(49.,-15.5857864376269,74.));
#8836=CARTESIAN_POINT('Origin',(49.,-15.5857864376269,75.));
#8837=CARTESIAN_POINT('',(49.,44.5857864376269,74.));
#8838=CARTESIAN_POINT('',(49.,-10.5,74.));
#8839=CARTESIAN_POINT('Origin',(49.,44.5857864376269,75.));
#8840=CARTESIAN_POINT('Origin',(15.6360389693211,-20.,75.));
#8841=CARTESIAN_POINT('',(44.5857864376269,-20.,74.));
#8842=CARTESIAN_POINT('',(15.6360389693211,-20.,74.));
#8843=CARTESIAN_POINT('',(45.,-21.,75.));
#8844=CARTESIAN_POINT('Origin',(44.5857864376269,-20.,75.));
#8845=CARTESIAN_POINT('',(15.6360389693211,-21.,75.));
#8846=CARTESIAN_POINT('Origin',(39.5428932188134,-25.0428932188135,75.));
#8847=CARTESIAN_POINT('',(40.25,-25.75,75.));
#8848=CARTESIAN_POINT('',(39.5428932188134,-25.0428932188135,74.));
#8849=CARTESIAN_POINT('Origin',(48.0428932188135,45.5428932188135,75.));
#8850=CARTESIAN_POINT('',(45.,50.,75.));
#8851=CARTESIAN_POINT('',(48.75,46.25,75.));
#8852=CARTESIAN_POINT('',(44.5857864376269,49.,74.));
#8853=CARTESIAN_POINT('',(48.0428932188135,45.5428932188135,74.));
#8854=CARTESIAN_POINT('Origin',(44.5857864376269,49.,75.));
#8855=CARTESIAN_POINT('Origin',(22.5,49.,75.));
#8856=CARTESIAN_POINT('',(-45.,50.,75.));
#8857=CARTESIAN_POINT('',(22.5,50.,75.));
#8858=CARTESIAN_POINT('',(-44.5857864376269,49.,74.));
#8859=CARTESIAN_POINT('',(22.5,49.,74.));
#8860=CARTESIAN_POINT('Origin',(-44.5857864376269,49.,75.));
#8861=CARTESIAN_POINT('Origin',(25.0428932188134,-39.5428932188134,75.));
#8862=CARTESIAN_POINT('',(25.0428932188134,-39.5428932188134,74.));
#8863=CARTESIAN_POINT('',(25.75,-40.25,75.));
#8864=CARTESIAN_POINT('Origin',(-45.5428932188135,48.0428932188135,75.));
#8865=CARTESIAN_POINT('',(-50.,45.,75.));
#8866=CARTESIAN_POINT('',(-46.25,48.75,75.));
#8867=CARTESIAN_POINT('',(-49.,44.5857864376269,74.));
#8868=CARTESIAN_POINT('',(-45.5428932188135,48.0428932188135,74.));
#8869=CARTESIAN_POINT('Origin',(-49.,44.5857864376269,75.));
#8870=CARTESIAN_POINT('Origin',(-49.,22.5,75.));
#8871=CARTESIAN_POINT('',(-50.,-45.,75.));
#8872=CARTESIAN_POINT('',(-50.,22.5,75.));
#8873=CARTESIAN_POINT('',(-49.,-44.5857864376269,74.));
#8874=CARTESIAN_POINT('',(-49.,22.5,74.));
#8875=CARTESIAN_POINT('Origin',(-49.,-44.5857864376269,75.));
#8876=CARTESIAN_POINT('Origin',(-48.0428932188135,-45.5428932188135,75.));
#8877=CARTESIAN_POINT('',(-48.75,-46.25,75.));
#8878=CARTESIAN_POINT('',(-48.0428932188135,-45.5428932188135,74.));
#8879=CARTESIAN_POINT('Origin',(18.5,-47.5,74.));
#8880=CARTESIAN_POINT('',(21.,-45.,85.));
#8881=CARTESIAN_POINT('',(21.,-45.,74.));
#8882=CARTESIAN_POINT('',(25.75,-40.25,85.));
#8883=CARTESIAN_POINT('',(16.,-50.,74.));
#8884=CARTESIAN_POINT('Origin',(21.,-50.,74.));
#8885=CARTESIAN_POINT('',(21.,-31.2720779386421,85.));
#8886=CARTESIAN_POINT('',(21.,-31.2720779386421,74.));
#8887=CARTESIAN_POINT('',(21.,-25.,85.));
#8888=CARTESIAN_POINT('Origin',(21.,-31.2720779386421,74.));
#8889=CARTESIAN_POINT('',(31.2720779386421,-21.,85.));
#8890=CARTESIAN_POINT('',(31.2720779386421,-21.,74.));
#8891=CARTESIAN_POINT('',(23.5680194846605,-28.7040584539816,85.));
#8892=CARTESIAN_POINT('Origin',(31.2720779386421,-21.,74.));
#8893=CARTESIAN_POINT('',(45.,-21.,85.));
#8894=CARTESIAN_POINT('',(45.,-21.,74.));
#8895=CARTESIAN_POINT('',(15.6360389693211,-21.,85.));
#8896=CARTESIAN_POINT('Origin',(47.5,-18.5,74.));
#8897=CARTESIAN_POINT('',(50.,-16.,85.));
#8898=CARTESIAN_POINT('',(50.,-16.,74.));
#8899=CARTESIAN_POINT('',(40.25,-25.75,85.));
#8900=CARTESIAN_POINT('Origin',(50.,-21.,74.));
#8901=CARTESIAN_POINT('',(50.,45.,85.));
#8902=CARTESIAN_POINT('',(50.,45.,74.));
#8903=CARTESIAN_POINT('',(50.,-10.5,85.));
#8904=CARTESIAN_POINT('Origin',(0.,0.,74.));
#8905=CARTESIAN_POINT('Origin',(-48.0428932188135,-45.5428932188135,85.));
#8906=CARTESIAN_POINT('',(-50.,-45.,85.));
#8907=CARTESIAN_POINT('Origin',(-49.,-44.5857864376269,85.));
#8908=CARTESIAN_POINT('',(-48.75,-46.25,85.));
#8909=CARTESIAN_POINT('Origin',(-49.,22.5,85.));
#8910=CARTESIAN_POINT('',(-50.,45.,85.));
#8911=CARTESIAN_POINT('Origin',(-49.,44.5857864376269,85.));
#8912=CARTESIAN_POINT('',(-50.,22.5,85.));
#8913=CARTESIAN_POINT('Origin',(-45.5428932188135,48.0428932188135,85.));
#8914=CARTESIAN_POINT('',(-46.25,48.75,85.));
#8915=CARTESIAN_POINT('Origin',(48.0428932188135,45.5428932188135,85.));
#8916=CARTESIAN_POINT('Origin',(49.,44.5857864376269,85.));
#8917=CARTESIAN_POINT('',(48.75,46.25,85.));
#8918=CARTESIAN_POINT('Origin',(49.,-10.5,85.));
#8919=CARTESIAN_POINT('Origin',(49.,-15.5857864376269,85.));
#8920=CARTESIAN_POINT('Origin',(39.5428932188134,-25.0428932188135,85.));
#8921=CARTESIAN_POINT('Origin',(44.5857864376269,-20.,85.));
#8922=CARTESIAN_POINT('Origin',(15.6360389693211,-20.,85.));
#8923=CARTESIAN_POINT('Origin',(30.857864376269,-20.,85.));
#8924=CARTESIAN_POINT('Origin',(22.860912703474,-27.9969516727951,85.));
#8925=CARTESIAN_POINT('Origin',(20.,-30.8578643762691,85.));
#8926=CARTESIAN_POINT('Origin',(20.,-25.,85.));
#8927=CARTESIAN_POINT('Origin',(20.,-44.5857864376269,85.));
#8928=CARTESIAN_POINT('Origin',(25.0428932188134,-39.5428932188134,85.));
#8929=CARTESIAN_POINT('Origin',(-45.,-50.,74.));
#8930=CARTESIAN_POINT('',(-45.,-50.,74.));
#8931=CARTESIAN_POINT('Origin',(-50.,-45.,74.));
#8932=CARTESIAN_POINT('',(-50.,-45.,74.));
#8933=CARTESIAN_POINT('Origin',(-50.,45.,74.));
#8934=CARTESIAN_POINT('',(-50.,45.,74.));
#8935=CARTESIAN_POINT('Origin',(-45.,50.,74.));
#8936=CARTESIAN_POINT('',(-45.,50.,74.));
#8937=CARTESIAN_POINT('Origin',(45.,50.,74.));
#8938=CARTESIAN_POINT('',(45.,50.,74.));
#8939=CARTESIAN_POINT('Origin',(50.,45.,74.));
#8940=CARTESIAN_POINT('',(0.,0.,0.));
#8941=CARTESIAN_POINT('Origin',(29.,-25.,21.));
#8942=CARTESIAN_POINT('',(30.,-35.,21.));
#8943=CARTESIAN_POINT('',(30.,-45.,21.));
#8944=CARTESIAN_POINT('',(30.,-25.,21.));
#8945=CARTESIAN_POINT('',(29.,-44.5857864376269,20.));
#8946=CARTESIAN_POINT('Origin',(29.,-44.5857864376269,21.));
#8947=CARTESIAN_POINT('',(29.,-34.5857864376269,20.));
#8948=CARTESIAN_POINT('',(29.,-25.,20.));
#8949=CARTESIAN_POINT('Origin',(29.,-34.5857864376269,21.));
#8950=CARTESIAN_POINT('Origin',(15.,-29.,21.));
#8951=CARTESIAN_POINT('',(34.5857864376269,-29.,20.));
#8952=CARTESIAN_POINT('',(44.5857864376269,-29.,20.));
#8953=CARTESIAN_POINT('',(15.,-29.,20.));
#8954=CARTESIAN_POINT('',(45.,-30.,21.));
#8955=CARTESIAN_POINT('Origin',(44.5857864376269,-29.,21.));
#8956=CARTESIAN_POINT('',(35.,-30.,21.));
#8957=CARTESIAN_POINT('',(15.,-30.,21.));
#8958=CARTESIAN_POINT('Origin',(34.5857864376269,-29.,21.));
#8959=CARTESIAN_POINT('Origin',(41.7928932188135,-31.7928932188135,21.));
#8960=CARTESIAN_POINT('',(49.,-24.5857864376269,20.));
#8961=CARTESIAN_POINT('',(41.7928932188135,-31.7928932188135,20.));
#8962=CARTESIAN_POINT('',(50.,-25.,21.));
#8963=CARTESIAN_POINT('Origin',(49.,-24.5857864376269,21.));
#8964=CARTESIAN_POINT('',(42.5,-32.5,21.));
#8965=CARTESIAN_POINT('Origin',(49.,-15.,21.));
#8966=CARTESIAN_POINT('',(49.,44.5857864376269,20.));
#8967=CARTESIAN_POINT('',(49.,-15.,20.));
#8968=CARTESIAN_POINT('',(50.,45.,21.));
#8969=CARTESIAN_POINT('Origin',(49.,44.5857864376269,21.));
#8970=CARTESIAN_POINT('',(50.,-15.,21.));
#8971=CARTESIAN_POINT('Origin',(46.7928932188135,46.7928932188135,21.));
#8972=CARTESIAN_POINT('',(44.5857864376269,49.,20.));
#8973=CARTESIAN_POINT('',(46.7928932188135,46.7928932188135,20.));
#8974=CARTESIAN_POINT('',(45.,50.,21.));
#8975=CARTESIAN_POINT('Origin',(44.5857864376269,49.,21.));
#8976=CARTESIAN_POINT('',(47.5,47.5,21.));
#8977=CARTESIAN_POINT('Origin',(25.,49.,21.));
#8978=CARTESIAN_POINT('',(-44.5857864376269,49.,20.));
#8979=CARTESIAN_POINT('',(25.,49.,20.));
#8980=CARTESIAN_POINT('',(-45.,50.,21.));
#8981=CARTESIAN_POINT('Origin',(-44.5857864376269,49.,21.));
#8982=CARTESIAN_POINT('',(25.,50.,21.));
#8983=CARTESIAN_POINT('Origin',(-46.7928932188135,46.7928932188135,21.));
#8984=CARTESIAN_POINT('',(-50.,45.,21.));
#8985=CARTESIAN_POINT('',(-47.5,47.5,21.));
#8986=CARTESIAN_POINT('',(-49.,44.5857864376269,20.));
#8987=CARTESIAN_POINT('',(-46.7928932188135,46.7928932188135,20.));
#8988=CARTESIAN_POINT('Origin',(-49.,44.5857864376269,21.));
#8989=CARTESIAN_POINT('Origin',(-49.,25.,21.));
#8990=CARTESIAN_POINT('',(-50.,-45.,21.));
#8991=CARTESIAN_POINT('',(-50.,25.,21.));
#8992=CARTESIAN_POINT('',(-49.,-44.5857864376269,20.));
#8993=CARTESIAN_POINT('',(-49.,25.,20.));
#8994=CARTESIAN_POINT('Origin',(-49.,-44.5857864376269,21.));
#8995=CARTESIAN_POINT('Origin',(-46.7928932188135,-46.7928932188135,21.));
#8996=CARTESIAN_POINT('',(-45.,-50.,21.));
#8997=CARTESIAN_POINT('',(-47.5,-47.5,21.));
#8998=CARTESIAN_POINT('',(-44.5857864376269,-49.,20.));
#8999=CARTESIAN_POINT('',(-46.7928932188135,-46.7928932188135,20.));
#9000=CARTESIAN_POINT('Origin',(-44.5857864376269,-49.,21.));
#9001=CARTESIAN_POINT('Origin',(-25.,-49.,21.));
#9002=CARTESIAN_POINT('',(25.,-50.,21.));
#9003=CARTESIAN_POINT('',(-25.,-50.,21.));
#9004=CARTESIAN_POINT('',(24.5857864376269,-49.,20.));
#9005=CARTESIAN_POINT('',(-25.,-49.,20.));
#9006=CARTESIAN_POINT('Origin',(24.5857864376269,-49.,21.));
#9007=CARTESIAN_POINT('Origin',(31.7928932188135,-41.7928932188135,21.));
#9008=CARTESIAN_POINT('',(32.5,-42.5,21.));
#9009=CARTESIAN_POINT('',(31.7928932188135,-41.7928932188135,20.));
#9010=CARTESIAN_POINT('Origin',(31.7928932188135,-31.7928932188135,21.));
#9011=CARTESIAN_POINT('',(32.5,-32.5,21.));
#9012=CARTESIAN_POINT('',(31.7928932188135,-31.7928932188135,20.));
#9013=CARTESIAN_POINT('Origin',(-47.5,-47.5,20.));
#9014=CARTESIAN_POINT('',(-45.,-50.,34.));
#9015=CARTESIAN_POINT('',(-45.,-50.,20.));
#9016=CARTESIAN_POINT('',(-50.,-45.,34.));
#9017=CARTESIAN_POINT('',(-47.5,-47.5,34.));
#9018=CARTESIAN_POINT('',(-50.,-45.,20.));
#9019=CARTESIAN_POINT('Origin',(-50.,-50.,20.));
#9020=CARTESIAN_POINT('',(25.,-50.,34.));
#9021=CARTESIAN_POINT('',(25.,-50.,20.));
#9022=CARTESIAN_POINT('',(-25.,-50.,34.));
#9023=CARTESIAN_POINT('Origin',(27.5,-47.5,20.));
#9024=CARTESIAN_POINT('',(30.,-45.,34.));
#9025=CARTESIAN_POINT('',(30.,-45.,20.));
#9026=CARTESIAN_POINT('',(32.5,-42.5,34.));
#9027=CARTESIAN_POINT('Origin',(30.,-50.,20.));
#9028=CARTESIAN_POINT('',(30.,-35.,34.));
#9029=CARTESIAN_POINT('',(30.,-35.,20.));
#9030=CARTESIAN_POINT('',(30.,-25.,34.));
#9031=CARTESIAN_POINT('Origin',(32.5,-32.5,20.));
#9032=CARTESIAN_POINT('',(35.,-30.,34.));
#9033=CARTESIAN_POINT('',(35.,-30.,20.));
#9034=CARTESIAN_POINT('',(32.5,-32.5,34.));
#9035=CARTESIAN_POINT('Origin',(30.,-30.,20.));
#9036=CARTESIAN_POINT('',(45.,-30.,34.));
#9037=CARTESIAN_POINT('',(45.,-30.,20.));
#9038=CARTESIAN_POINT('',(15.,-30.,34.));
#9039=CARTESIAN_POINT('Origin',(0.,0.,20.));
#9040=CARTESIAN_POINT('Origin',(29.,-25.,34.));
#9041=CARTESIAN_POINT('',(29.,-34.5857864376269,35.));
#9042=CARTESIAN_POINT('',(29.,-44.5857864376269,35.));
#9043=CARTESIAN_POINT('',(29.,-25.,35.));
#9044=CARTESIAN_POINT('Origin',(29.,-44.5857864376269,34.));
#9045=CARTESIAN_POINT('Origin',(29.,-34.5857864376269,34.));
#9046=CARTESIAN_POINT('Origin',(31.7928932188135,-41.7928932188135,34.));
#9047=CARTESIAN_POINT('',(24.5857864376269,-49.,35.));
#9048=CARTESIAN_POINT('',(31.7928932188135,-41.7928932188135,35.));
#9049=CARTESIAN_POINT('Origin',(24.5857864376269,-49.,34.));
#9050=CARTESIAN_POINT('Origin',(-25.,-49.,34.));
#9051=CARTESIAN_POINT('',(-44.5857864376269,-49.,35.));
#9052=CARTESIAN_POINT('',(-25.,-49.,35.));
#9053=CARTESIAN_POINT('Origin',(-44.5857864376269,-49.,34.));
#9054=CARTESIAN_POINT('Origin',(-46.7928932188135,-46.7928932188135,34.));
#9055=CARTESIAN_POINT('',(-49.,-44.5857864376269,35.));
#9056=CARTESIAN_POINT('',(-46.7928932188135,-46.7928932188135,35.));
#9057=CARTESIAN_POINT('Origin',(-49.,-44.5857864376269,34.));
#9058=CARTESIAN_POINT('Origin',(-49.,25.,34.));
#9059=CARTESIAN_POINT('',(-49.,44.5857864376269,35.));
#9060=CARTESIAN_POINT('',(-49.,25.,35.));
#9061=CARTESIAN_POINT('',(-50.,45.,34.));
#9062=CARTESIAN_POINT('Origin',(-49.,44.5857864376269,34.));
#9063=CARTESIAN_POINT('',(-50.,25.,34.));
#9064=CARTESIAN_POINT('Origin',(-46.7928932188135,46.7928932188135,34.));
#9065=CARTESIAN_POINT('',(-45.,50.,34.));
#9066=CARTESIAN_POINT('',(-47.5,47.5,34.));
#9067=CARTESIAN_POINT('',(-44.5857864376269,49.,35.));
#9068=CARTESIAN_POINT('',(-46.7928932188135,46.7928932188135,35.));
#9069=CARTESIAN_POINT('Origin',(-44.5857864376269,49.,34.));
#9070=CARTESIAN_POINT('Origin',(25.,49.,34.));
#9071=CARTESIAN_POINT('',(45.,50.,34.));
#9072=CARTESIAN_POINT('',(25.,50.,34.));
#9073=CARTESIAN_POINT('',(44.5857864376269,49.,35.));
#9074=CARTESIAN_POINT('',(25.,49.,35.));
#9075=CARTESIAN_POINT('Origin',(44.5857864376269,49.,34.));
#9076=CARTESIAN_POINT('Origin',(46.7928932188135,46.7928932188135,34.));
#9077=CARTESIAN_POINT('',(50.,45.,34.));
#9078=CARTESIAN_POINT('',(47.5,47.5,34.));
#9079=CARTESIAN_POINT('',(49.,44.5857864376269,35.));
#9080=CARTESIAN_POINT('',(46.7928932188135,46.7928932188135,35.));
#9081=CARTESIAN_POINT('Origin',(49.,44.5857864376269,34.));
#9082=CARTESIAN_POINT('Origin',(49.,-15.,34.));
#9083=CARTESIAN_POINT('',(50.,-25.,34.));
#9084=CARTESIAN_POINT('',(50.,-15.,34.));
#9085=CARTESIAN_POINT('',(49.,-24.5857864376269,35.));
#9086=CARTESIAN_POINT('',(49.,-15.,35.));
#9087=CARTESIAN_POINT('Origin',(49.,-24.5857864376269,34.));
#9088=CARTESIAN_POINT('Origin',(41.7928932188135,-31.7928932188135,34.));
#9089=CARTESIAN_POINT('',(42.5,-32.5,34.));
#9090=CARTESIAN_POINT('',(44.5857864376269,-29.,35.));
#9091=CARTESIAN_POINT('',(41.7928932188135,-31.7928932188135,35.));
#9092=CARTESIAN_POINT('Origin',(44.5857864376269,-29.,34.));
#9093=CARTESIAN_POINT('Origin',(15.,-29.,34.));
#9094=CARTESIAN_POINT('',(34.5857864376269,-29.,35.));
#9095=CARTESIAN_POINT('',(15.,-29.,35.));
#9096=CARTESIAN_POINT('Origin',(34.5857864376269,-29.,34.));
#9097=CARTESIAN_POINT('Origin',(31.7928932188135,-31.7928932188135,34.));
#9098=CARTESIAN_POINT('',(31.7928932188135,-31.7928932188135,35.));
#9099=CARTESIAN_POINT('Origin',(47.5,47.5,20.));
#9100=CARTESIAN_POINT('',(45.,50.,20.));
#9101=CARTESIAN_POINT('',(50.,45.,20.));
#9102=CARTESIAN_POINT('Origin',(50.,-30.,20.));
#9103=CARTESIAN_POINT('',(50.,-25.,20.));
#9104=CARTESIAN_POINT('Origin',(47.5,-27.5,20.));
#9105=CARTESIAN_POINT('Origin',(0.,0.,35.));
#9106=CARTESIAN_POINT('Origin',(-47.5,47.5,20.));
#9107=CARTESIAN_POINT('',(-50.,45.,20.));
#9108=CARTESIAN_POINT('',(-45.,50.,20.));
#9109=CARTESIAN_POINT('Origin',(50.,50.,20.));
#9110=CARTESIAN_POINT('Origin',(-50.,50.,20.));
#9111=CARTESIAN_POINT('',(0.,0.,0.));
#9112=CARTESIAN_POINT('Origin',(21.2760503877808,-85.,85.));
#9113=CARTESIAN_POINT('',(18.2760503877808,-82.,85.));
#9114=CARTESIAN_POINT('Origin',(21.2760503877808,-82.,85.));
#9115=CARTESIAN_POINT('',(18.2760503877808,-66.,85.));
#9116=CARTESIAN_POINT('',(18.2760503877808,-85.,85.));
#9117=CARTESIAN_POINT('Origin',(21.2760503877808,-66.,85.));
#9118=CARTESIAN_POINT('Origin',(-20.7760503877808,-85.,85.));
#9119=CARTESIAN_POINT('',(-23.7760503877808,-82.,85.));
#9120=CARTESIAN_POINT('Origin',(-20.7760503877808,-82.,85.));
#9121=CARTESIAN_POINT('',(-23.7760503877808,-66.,85.));
#9122=CARTESIAN_POINT('',(-23.7760503877808,-85.,85.));
#9123=CARTESIAN_POINT('Origin',(-20.7760503877808,-66.,85.));
#9124=CARTESIAN_POINT('Origin',(-42.1783940322367,-82.,71.1256934864884));
#9125=CARTESIAN_POINT('',(-45.1783940322367,-82.,71.1256934864884));
#9126=CARTESIAN_POINT('Origin',(-42.1783940322367,-82.,71.1256934864884));
#9127=CARTESIAN_POINT('',(-45.1783940322367,-66.,71.1256934864884));
#9128=CARTESIAN_POINT('',(-45.1783940322367,-82.,71.1256934864884));
#9129=CARTESIAN_POINT('Origin',(-42.1783940322367,-66.,71.1256934864884));
#9130=CARTESIAN_POINT('Origin',(42.6783940322367,-82.,97.7923601531551));
#9131=CARTESIAN_POINT('',(39.6783940322367,-82.,97.7923601531551));
#9132=CARTESIAN_POINT('Origin',(42.6783940322367,-82.,97.7923601531551));
#9133=CARTESIAN_POINT('',(39.6783940322367,-66.,97.7923601531551));
#9134=CARTESIAN_POINT('',(39.6783940322367,-82.,97.7923601531551));
#9135=CARTESIAN_POINT('Origin',(42.6783940322367,-66.,97.7923601531551));
#9136=CARTESIAN_POINT('Origin',(42.6783940322367,-82.,71.1256934864884));
#9137=CARTESIAN_POINT('',(39.6783940322367,-82.,71.1256934864884));
#9138=CARTESIAN_POINT('Origin',(42.6783940322367,-82.,71.1256934864884));
#9139=CARTESIAN_POINT('',(39.6783940322367,-66.,71.1256934864884));
#9140=CARTESIAN_POINT('',(39.6783940322367,-82.,71.1256934864884));
#9141=CARTESIAN_POINT('Origin',(42.6783940322367,-66.,71.1256934864884));
#9142=CARTESIAN_POINT('Origin',(-42.1783940322367,-82.,97.7923601531551));
#9143=CARTESIAN_POINT('',(-45.1783940322367,-82.,97.7923601531551));
#9144=CARTESIAN_POINT('Origin',(-42.1783940322367,-82.,97.7923601531551));
#9145=CARTESIAN_POINT('',(-45.1783940322367,-66.,97.7923601531551));
#9146=CARTESIAN_POINT('',(-45.1783940322367,-82.,97.7923601531551));
#9147=CARTESIAN_POINT('Origin',(-42.1783940322367,-66.,97.7923601531551));
#9148=CARTESIAN_POINT('Origin',(-42.1783940322367,-82.,44.4590268198217));
#9149=CARTESIAN_POINT('',(-45.1783940322367,-82.,44.4590268198217));
#9150=CARTESIAN_POINT('Origin',(-42.1783940322367,-82.,44.4590268198217));
#9151=CARTESIAN_POINT('',(-45.1783940322367,-66.,44.4590268198217));
#9152=CARTESIAN_POINT('',(-45.1783940322367,-82.,44.4590268198217));
#9153=CARTESIAN_POINT('Origin',(-42.1783940322367,-66.,44.4590268198217));
#9154=CARTESIAN_POINT('Origin',(42.6783940322367,-82.,124.459026819822));
#9155=CARTESIAN_POINT('',(39.6783940322367,-82.,124.459026819822));
#9156=CARTESIAN_POINT('Origin',(42.6783940322367,-82.,124.459026819822));
#9157=CARTESIAN_POINT('',(39.6783940322367,-66.,124.459026819822));
#9158=CARTESIAN_POINT('',(39.6783940322367,-82.,124.459026819822));
#9159=CARTESIAN_POINT('Origin',(42.6783940322367,-66.,124.459026819822));
#9160=CARTESIAN_POINT('Origin',(42.6783940322367,-82.,44.4590268198217));
#9161=CARTESIAN_POINT('',(39.6783940322367,-82.,44.4590268198217));
#9162=CARTESIAN_POINT('Origin',(42.6783940322367,-82.,44.4590268198217));
#9163=CARTESIAN_POINT('',(39.6783940322367,-66.,44.4590268198217));
#9164=CARTESIAN_POINT('',(39.6783940322367,-82.,44.4590268198217));
#9165=CARTESIAN_POINT('Origin',(42.6783940322367,-66.,44.4590268198217));
#9166=CARTESIAN_POINT('Origin',(-42.1783940322367,-82.,124.459026819822));
#9167=CARTESIAN_POINT('',(-45.1783940322367,-82.,124.459026819822));
#9168=CARTESIAN_POINT('Origin',(-42.1783940322367,-82.,124.459026819822));
#9169=CARTESIAN_POINT('',(-45.1783940322367,-66.,124.459026819822));
#9170=CARTESIAN_POINT('',(-45.1783940322367,-82.,124.459026819822));
#9171=CARTESIAN_POINT('Origin',(-42.1783940322367,-66.,124.459026819822));
#9172=CARTESIAN_POINT('Origin',(49.5,-67.,60.));
#9173=CARTESIAN_POINT('',(50.5,-67.,130.));
#9174=CARTESIAN_POINT('',(50.5,-67.,40.));
#9175=CARTESIAN_POINT('',(50.5,-67.,60.));
#9176=CARTESIAN_POINT('',(49.5,-66.,40.4142135623731));
#9177=CARTESIAN_POINT('Origin',(49.5,-67.,40.4142135623731));
#9178=CARTESIAN_POINT('',(49.5,-66.,129.585786437627));
#9179=CARTESIAN_POINT('',(49.5,-66.,60.));
#9180=CARTESIAN_POINT('Origin',(49.5,-67.,129.585786437627));
#9181=CARTESIAN_POINT('Origin',(47.2928932188134,-67.,38.2071067811866));
#9182=CARTESIAN_POINT('',(45.5,-67.,35.));
#9183=CARTESIAN_POINT('',(48.,-67.,37.5));
#9184=CARTESIAN_POINT('',(45.0857864376269,-66.,36.));
#9185=CARTESIAN_POINT('Origin',(45.0857864376269,-67.,36.));
#9186=CARTESIAN_POINT('',(47.2928932188134,-66.,38.2071067811866));
#9187=CARTESIAN_POINT('Origin',(-24.5,-67.,36.));
#9188=CARTESIAN_POINT('',(-45.,-67.,35.));
#9189=CARTESIAN_POINT('',(-24.5,-67.,35.));
#9190=CARTESIAN_POINT('',(-44.5857864376269,-66.,36.));
#9191=CARTESIAN_POINT('Origin',(-44.5857864376269,-67.,36.));
#9192=CARTESIAN_POINT('',(-24.5,-66.,36.));
#9193=CARTESIAN_POINT('Origin',(-46.6678932188135,-67.,38.0821067811865));
#9194=CARTESIAN_POINT('',(-50.,-67.,40.));
#9195=CARTESIAN_POINT('',(-47.375,-67.,37.375));
#9196=CARTESIAN_POINT('',(-49.,-66.,40.4142135623731));
#9197=CARTESIAN_POINT('Origin',(-49.,-67.,40.4142135623731));
#9198=CARTESIAN_POINT('',(-46.6678932188135,-66.,38.0821067811865));
#9199=CARTESIAN_POINT('Origin',(-49.,-67.,110.));
#9200=CARTESIAN_POINT('',(-49.,-66.,129.585786437627));
#9201=CARTESIAN_POINT('',(-49.,-66.,110.));
#9202=CARTESIAN_POINT('',(-50.,-67.,130.));
#9203=CARTESIAN_POINT('',(-50.,-67.,110.));
#9204=CARTESIAN_POINT('Origin',(-49.,-67.,129.585786437627));
#9205=CARTESIAN_POINT('Origin',(-46.6678932188135,-67.,131.917893218813));
#9206=CARTESIAN_POINT('',(-44.5857864376269,-66.,134.));
#9207=CARTESIAN_POINT('',(-46.6678932188135,-66.,131.917893218813));
#9208=CARTESIAN_POINT('',(-45.,-67.,135.));
#9209=CARTESIAN_POINT('',(-47.375,-67.,132.625));
#9210=CARTESIAN_POINT('Origin',(-44.5857864376269,-67.,134.));
#9211=CARTESIAN_POINT('Origin',(25.5,-67.,134.));
#9212=CARTESIAN_POINT('',(45.0857864376269,-66.,134.));
#9213=CARTESIAN_POINT('',(25.5,-66.,134.));
#9214=CARTESIAN_POINT('',(45.5,-67.,135.));
#9215=CARTESIAN_POINT('',(25.5,-67.,135.));
#9216=CARTESIAN_POINT('Origin',(45.0857864376269,-67.,134.));
#9217=CARTESIAN_POINT('Origin',(47.2928932188134,-67.,131.792893218813));
#9218=CARTESIAN_POINT('',(48.,-67.,132.5));
#9219=CARTESIAN_POINT('',(47.2928932188134,-66.,131.792893218813));
#9220=CARTESIAN_POINT('Origin',(-47.5,-66.,37.5));
#9221=CARTESIAN_POINT('',(-45.,-81.,35.));
#9222=CARTESIAN_POINT('',(-45.,-66.,35.));
#9223=CARTESIAN_POINT('',(-50.,-81.,40.));
#9224=CARTESIAN_POINT('',(-47.375,-81.,37.375));
#9225=CARTESIAN_POINT('',(-50.,-66.,40.));
#9226=CARTESIAN_POINT('Origin',(-49.5,-66.,35.));
#9227=CARTESIAN_POINT('',(45.5,-81.,35.));
#9228=CARTESIAN_POINT('',(45.5,-66.,35.));
#9229=CARTESIAN_POINT('',(-24.5,-81.,35.));
#9230=CARTESIAN_POINT('Origin',(48.,-66.,37.5));
#9231=CARTESIAN_POINT('',(50.5,-81.,40.));
#9232=CARTESIAN_POINT('',(50.5,-66.,40.));
#9233=CARTESIAN_POINT('',(48.,-81.,37.5));
#9234=CARTESIAN_POINT('Origin',(50.5,-66.,35.));
#9235=CARTESIAN_POINT('',(50.5,-81.,130.));
#9236=CARTESIAN_POINT('',(50.5,-66.,130.));
#9237=CARTESIAN_POINT('',(50.5,-81.,60.));
#9238=CARTESIAN_POINT('Origin',(0.499999999999998,-66.,85.));
#9239=CARTESIAN_POINT('Origin',(49.5,-81.,60.));
#9240=CARTESIAN_POINT('',(49.5,-82.,129.585786437627));
#9241=CARTESIAN_POINT('',(49.5,-82.,40.4142135623731));
#9242=CARTESIAN_POINT('',(49.5,-82.,60.));
#9243=CARTESIAN_POINT('Origin',(49.5,-81.,40.4142135623731));
#9244=CARTESIAN_POINT('Origin',(49.5,-81.,129.585786437627));
#9245=CARTESIAN_POINT('Origin',(47.2928932188134,-81.,38.2071067811866));
#9246=CARTESIAN_POINT('',(45.0857864376269,-82.,36.));
#9247=CARTESIAN_POINT('',(47.2928932188134,-82.,38.2071067811866));
#9248=CARTESIAN_POINT('Origin',(45.0857864376269,-81.,36.));
#9249=CARTESIAN_POINT('Origin',(-24.5,-81.,36.));
#9250=CARTESIAN_POINT('',(-44.5857864376269,-82.,36.));
#9251=CARTESIAN_POINT('',(-24.5,-82.,36.));
#9252=CARTESIAN_POINT('Origin',(-44.5857864376269,-81.,36.));
#9253=CARTESIAN_POINT('Origin',(-46.6678932188135,-81.,38.0821067811865));
#9254=CARTESIAN_POINT('',(-49.,-82.,40.4142135623731));
#9255=CARTESIAN_POINT('',(-46.6678932188135,-82.,38.0821067811865));
#9256=CARTESIAN_POINT('Origin',(-49.,-81.,40.4142135623731));
#9257=CARTESIAN_POINT('Origin',(-49.,-81.,110.));
#9258=CARTESIAN_POINT('',(-50.,-81.,130.));
#9259=CARTESIAN_POINT('',(-50.,-81.,110.));
#9260=CARTESIAN_POINT('',(-49.,-82.,129.585786437627));
#9261=CARTESIAN_POINT('',(-49.,-82.,110.));
#9262=CARTESIAN_POINT('Origin',(-49.,-81.,129.585786437627));
#9263=CARTESIAN_POINT('Origin',(-46.6678932188135,-81.,131.917893218813));
#9264=CARTESIAN_POINT('',(-45.,-81.,135.));
#9265=CARTESIAN_POINT('',(-47.375,-81.,132.625));
#9266=CARTESIAN_POINT('',(-44.5857864376269,-82.,134.));
#9267=CARTESIAN_POINT('',(-46.6678932188135,-82.,131.917893218813));
#9268=CARTESIAN_POINT('Origin',(-44.5857864376269,-81.,134.));
#9269=CARTESIAN_POINT('Origin',(25.5,-81.,134.));
#9270=CARTESIAN_POINT('',(45.5,-81.,135.));
#9271=CARTESIAN_POINT('',(25.5,-81.,135.));
#9272=CARTESIAN_POINT('',(45.0857864376269,-82.,134.));
#9273=CARTESIAN_POINT('',(25.5,-82.,134.));
#9274=CARTESIAN_POINT('Origin',(45.0857864376269,-81.,134.));
#9275=CARTESIAN_POINT('Origin',(47.2928932188134,-81.,131.792893218813));
#9276=CARTESIAN_POINT('',(48.,-81.,132.5));
#9277=CARTESIAN_POINT('',(47.2928932188134,-82.,131.792893218813));
#9278=CARTESIAN_POINT('Origin',(-47.5,-66.,132.5));
#9279=CARTESIAN_POINT('',(-50.,-66.,130.));
#9280=CARTESIAN_POINT('',(-45.,-66.,135.));
#9281=CARTESIAN_POINT('Origin',(50.5,-66.,135.));
#9282=CARTESIAN_POINT('',(45.5,-66.,135.));
#9283=CARTESIAN_POINT('Origin',(48.,-66.,132.5));
#9284=CARTESIAN_POINT('Origin',(0.499999999999998,-82.,85.));
#9285=CARTESIAN_POINT('Origin',(-50.,-66.,135.));
#9286=CARTESIAN_POINT('',(0.,0.,0.));
#9287=CARTESIAN_POINT('Origin',(21.2760503877808,-85.,85.));
#9288=CARTESIAN_POINT('',(18.2760503877808,-85.,85.));
#9289=CARTESIAN_POINT('Origin',(21.2760503877808,-85.,85.));
#9290=CARTESIAN_POINT('',(18.2760503877808,-82.,85.));
#9291=CARTESIAN_POINT('',(18.2760503877808,-85.,85.));
#9292=CARTESIAN_POINT('Origin',(21.2760503877808,-82.,85.));
#9293=CARTESIAN_POINT('Origin',(-20.7760503877808,-85.,85.));
#9294=CARTESIAN_POINT('',(-23.7760503877808,-85.,85.));
#9295=CARTESIAN_POINT('Origin',(-20.7760503877808,-85.,85.));
#9296=CARTESIAN_POINT('',(-23.7760503877808,-82.,85.));
#9297=CARTESIAN_POINT('',(-23.7760503877808,-85.,85.));
#9298=CARTESIAN_POINT('Origin',(-20.7760503877808,-82.,85.));
#9299=CARTESIAN_POINT('Origin',(0.249999999999999,-96.1435033236749,79.));
#9300=CARTESIAN_POINT('',(2.24999999999999,-110.28700664735,79.));
#9301=CARTESIAN_POINT('',(-1.75000000000001,-110.28700664735,79.));
#9302=CARTESIAN_POINT('',(0.249999999999995,-110.28700664735,79.));
#9303=CARTESIAN_POINT('',(-8.80210077556162,-85.,79.));
#9304=CARTESIAN_POINT('',(-1.75000000000001,-110.28700664735,79.));
#9305=CARTESIAN_POINT('',(-32.75,-85.,79.));
#9306=CARTESIAN_POINT('',(-32.75,-85.,79.));
#9307=CARTESIAN_POINT('',(-32.75,-82.,79.));
#9308=CARTESIAN_POINT('',(-32.75,-79.,79.));
#9309=CARTESIAN_POINT('',(33.25,-82.,79.));
#9310=CARTESIAN_POINT('',(-44.5857864376269,-82.,79.));
#9311=CARTESIAN_POINT('',(33.25,-85.,79.));
#9312=CARTESIAN_POINT('',(33.25,-85.,79.));
#9313=CARTESIAN_POINT('',(9.30210077556161,-85.,79.));
#9314=CARTESIAN_POINT('',(-32.75,-85.,79.));
#9315=CARTESIAN_POINT('',(2.24999999999999,-110.28700664735,79.));
#9316=CARTESIAN_POINT('Origin',(-8.80210077556162,-85.,85.));
#9317=CARTESIAN_POINT('',(-1.75000000000001,-110.28700664735,91.));
#9318=CARTESIAN_POINT('',(-1.75000000000001,-110.28700664735,85.));
#9319=CARTESIAN_POINT('',(-8.80210077556162,-85.,91.));
#9320=CARTESIAN_POINT('',(-1.75000000000001,-110.28700664735,91.));
#9321=CARTESIAN_POINT('',(-8.80210077556162,-85.,85.));
#9322=CARTESIAN_POINT('Origin',(-32.75,-85.,85.));
#9323=CARTESIAN_POINT('',(-32.75,-85.,91.));
#9324=CARTESIAN_POINT('',(-32.75,-85.,91.));
#9325=CARTESIAN_POINT('',(-32.75,-85.,85.));
#9326=CARTESIAN_POINT('Origin',(-32.75,-82.,85.));
#9327=CARTESIAN_POINT('',(-32.75,-82.,91.));
#9328=CARTESIAN_POINT('',(-32.75,-79.,91.));
#9329=CARTESIAN_POINT('',(-32.75,-82.,85.));
#9330=CARTESIAN_POINT('Origin',(33.25,-82.,85.));
#9331=CARTESIAN_POINT('',(33.25,-82.,91.));
#9332=CARTESIAN_POINT('',(-44.5857864376269,-82.,91.));
#9333=CARTESIAN_POINT('',(33.25,-82.,85.));
#9334=CARTESIAN_POINT('Origin',(33.25,-85.,85.));
#9335=CARTESIAN_POINT('',(33.25,-85.,91.));
#9336=CARTESIAN_POINT('',(33.25,-85.,91.));
#9337=CARTESIAN_POINT('',(33.25,-85.,85.));
#9338=CARTESIAN_POINT('Origin',(9.30210077556162,-85.,85.));
#9339=CARTESIAN_POINT('',(9.30210077556161,-85.,91.));
#9340=CARTESIAN_POINT('',(-32.75,-85.,91.));
#9341=CARTESIAN_POINT('',(9.30210077556161,-85.,85.));
#9342=CARTESIAN_POINT('Origin',(2.24999999999999,-110.28700664735,85.));
#9343=CARTESIAN_POINT('',(2.24999999999999,-110.28700664735,91.));
#9344=CARTESIAN_POINT('',(2.24999999999999,-110.28700664735,91.));
#9345=CARTESIAN_POINT('',(2.24999999999999,-110.28700664735,85.));
#9346=CARTESIAN_POINT('Origin',(-1.75000000000001,-110.28700664735,85.));
#9347=CARTESIAN_POINT('',(0.249999999999995,-110.28700664735,91.));
#9348=CARTESIAN_POINT('Origin',(0.249999999999999,-96.1435033236749,91.));
#9349=CARTESIAN_POINT('',(0.,0.,0.));
#9350=CARTESIAN_POINT('Origin',(24.1186927691616,-58.,139.));
#9351=CARTESIAN_POINT('',(27.1186927691616,-58.,139.));
#9352=CARTESIAN_POINT('Origin',(24.1186927691616,-58.,139.));
#9353=CARTESIAN_POINT('',(27.1186927691616,-58.,135.));
#9354=CARTESIAN_POINT('',(27.1186927691616,-58.,139.));
#9355=CARTESIAN_POINT('Origin',(24.1186927691616,-58.,135.));
#9356=CARTESIAN_POINT('Origin',(24.1186927691616,-58.,135.));
#9357=CARTESIAN_POINT('Origin',(0.118692769161641,-58.,139.));
#9358=CARTESIAN_POINT('',(3.11869276916164,-58.,139.));
#9359=CARTESIAN_POINT('Origin',(0.118692769161641,-58.,139.));
#9360=CARTESIAN_POINT('',(3.11869276916164,-58.,135.));
#9361=CARTESIAN_POINT('',(3.11869276916164,-58.,139.));
#9362=CARTESIAN_POINT('Origin',(0.118692769161641,-58.,135.));
#9363=CARTESIAN_POINT('Origin',(0.118692769161641,-58.,135.));
#9364=CARTESIAN_POINT('Origin',(-23.8813072308384,-58.,139.));
#9365=CARTESIAN_POINT('',(-20.8813072308384,-58.,139.));
#9366=CARTESIAN_POINT('Origin',(-23.8813072308384,-58.,139.));
#9367=CARTESIAN_POINT('',(-20.8813072308384,-58.,135.));
#9368=CARTESIAN_POINT('',(-20.8813072308384,-58.,139.));
#9369=CARTESIAN_POINT('Origin',(-23.8813072308384,-58.,135.));
#9370=CARTESIAN_POINT('Origin',(-23.8813072308384,-58.,135.));
#9371=CARTESIAN_POINT('Origin',(-16.125,-64.,137.));
#9372=CARTESIAN_POINT('',(31.25,-64.,139.));
#9373=CARTESIAN_POINT('',(-30.75,-64.,139.));
#9374=CARTESIAN_POINT('',(-16.125,-64.,139.));
#9375=CARTESIAN_POINT('',(-32.75,-66.,137.));
#9376=CARTESIAN_POINT('Origin',(-30.75,-64.,137.));
#9377=CARTESIAN_POINT('',(33.25,-66.,137.));
#9378=CARTESIAN_POINT('',(-16.125,-66.,137.));
#9379=CARTESIAN_POINT('Origin',(31.25,-64.,137.));
#9380=CARTESIAN_POINT('Origin',(-30.75,-66.,137.));
#9381=CARTESIAN_POINT('',(-32.75,-50.,137.));
#9382=CARTESIAN_POINT('',(-32.75,-66.,137.));
#9383=CARTESIAN_POINT('',(-30.75,-52.,139.));
#9384=CARTESIAN_POINT('',(-30.75,-66.,139.));
#9385=CARTESIAN_POINT('Origin',(-30.75,-52.,137.));
#9386=CARTESIAN_POINT('Origin',(31.25,-66.,137.));
#9387=CARTESIAN_POINT('',(31.25,-52.,139.));
#9388=CARTESIAN_POINT('',(31.25,-66.,139.));
#9389=CARTESIAN_POINT('',(33.25,-50.,137.));
#9390=CARTESIAN_POINT('',(33.25,-66.,137.));
#9391=CARTESIAN_POINT('Origin',(31.25,-52.,137.));
#9392=CARTESIAN_POINT('Origin',(-16.125,-52.,137.));
#9393=CARTESIAN_POINT('',(-16.125,-50.,137.));
#9394=CARTESIAN_POINT('',(-16.125,-52.,139.));
#9395=CARTESIAN_POINT('Origin',(33.25,-66.,139.));
#9396=CARTESIAN_POINT('',(33.25,-66.,134.));
#9397=CARTESIAN_POINT('',(33.25,-66.,139.));
#9398=CARTESIAN_POINT('',(33.25,-65.,135.));
#9399=CARTESIAN_POINT('Origin',(33.25,-65.,134.));
#9400=CARTESIAN_POINT('',(33.25,-51.,135.));
#9401=CARTESIAN_POINT('',(33.25,-58.,135.));
#9402=CARTESIAN_POINT('',(33.25,-50.,134.));
#9403=CARTESIAN_POINT('Origin',(33.25,-51.,134.));
#9404=CARTESIAN_POINT('',(33.25,-50.,139.));
#9405=CARTESIAN_POINT('Origin',(0.499999999999998,-66.,85.));
#9406=CARTESIAN_POINT('',(-32.75,-66.,134.));
#9407=CARTESIAN_POINT('',(-32.75,-66.,129.));
#9408=CARTESIAN_POINT('',(-44.5857864376269,-66.,134.));
#9409=CARTESIAN_POINT('',(25.5,-66.,134.));
#9410=CARTESIAN_POINT('',(-49.,-66.,129.585786437627));
#9411=CARTESIAN_POINT('',(-46.6678932188135,-66.,131.917893218813));
#9412=CARTESIAN_POINT('',(-49.,-66.,40.4142135623731));
#9413=CARTESIAN_POINT('',(-49.,-66.,110.));
#9414=CARTESIAN_POINT('',(-44.5857864376269,-66.,36.));
#9415=CARTESIAN_POINT('',(-46.6678932188135,-66.,38.0821067811865));
#9416=CARTESIAN_POINT('',(45.0857864376269,-66.,36.));
#9417=CARTESIAN_POINT('',(-24.5,-66.,36.));
#9418=CARTESIAN_POINT('',(49.5,-66.,40.4142135623731));
#9419=CARTESIAN_POINT('',(47.2928932188134,-66.,38.2071067811866));
#9420=CARTESIAN_POINT('',(49.5,-66.,129.585786437627));
#9421=CARTESIAN_POINT('',(49.5,-66.,60.));
#9422=CARTESIAN_POINT('',(45.0857864376269,-66.,134.));
#9423=CARTESIAN_POINT('',(47.2928932188134,-66.,131.792893218813));
#9424=CARTESIAN_POINT('',(25.5,-66.,134.));
#9425=CARTESIAN_POINT('Origin',(-32.75,-66.,139.));
#9426=CARTESIAN_POINT('Origin',(-32.75,-66.,129.));
#9427=CARTESIAN_POINT('',(-32.75,-50.,134.));
#9428=CARTESIAN_POINT('',(-32.75,-50.,129.));
#9429=CARTESIAN_POINT('',(-32.75,-51.,135.));
#9430=CARTESIAN_POINT('Origin',(-32.75,-51.,134.));
#9431=CARTESIAN_POINT('',(-32.75,-65.,135.));
#9432=CARTESIAN_POINT('',(-32.75,-58.,135.));
#9433=CARTESIAN_POINT('Origin',(-32.75,-65.,134.));
#9434=CARTESIAN_POINT('Origin',(0.499999999999998,-50.,85.));
#9435=CARTESIAN_POINT('',(45.0857864376269,-50.,134.));
#9436=CARTESIAN_POINT('',(25.5,-50.,134.));
#9437=CARTESIAN_POINT('',(49.5,-50.,129.585786437627));
#9438=CARTESIAN_POINT('',(47.2928932188134,-50.,131.792893218813));
#9439=CARTESIAN_POINT('',(49.5,-50.,40.4142135623731));
#9440=CARTESIAN_POINT('',(49.5,-50.,60.));
#9441=CARTESIAN_POINT('',(45.0857864376269,-50.,36.));
#9442=CARTESIAN_POINT('',(47.2928932188134,-50.,38.2071067811866));
#9443=CARTESIAN_POINT('',(-44.5857864376269,-50.,36.));
#9444=CARTESIAN_POINT('',(-24.5,-50.,36.));
#9445=CARTESIAN_POINT('',(-49.,-50.,40.4142135623731));
#9446=CARTESIAN_POINT('',(-46.6678932188135,-50.,38.0821067811865));
#9447=CARTESIAN_POINT('',(-49.,-50.,129.585786437627));
#9448=CARTESIAN_POINT('',(-49.,-50.,110.));
#9449=CARTESIAN_POINT('',(-44.5857864376269,-50.,134.));
#9450=CARTESIAN_POINT('',(-46.6678932188135,-50.,131.917893218813));
#9451=CARTESIAN_POINT('',(25.5,-50.,134.));
#9452=CARTESIAN_POINT('Origin',(25.5,-51.,134.));
#9453=CARTESIAN_POINT('',(45.5,-51.,135.));
#9454=CARTESIAN_POINT('',(25.5,-51.,135.));
#9455=CARTESIAN_POINT('Origin',(45.0857864376269,-51.,134.));
#9456=CARTESIAN_POINT('Origin',(25.5,-51.,134.));
#9457=CARTESIAN_POINT('',(-45.,-51.,135.));
#9458=CARTESIAN_POINT('Origin',(-44.5857864376269,-51.,134.));
#9459=CARTESIAN_POINT('',(25.5,-51.,135.));
#9460=CARTESIAN_POINT('Origin',(50.5,-50.,135.));
#9461=CARTESIAN_POINT('',(45.5,-65.,135.));
#9462=CARTESIAN_POINT('',(25.5,-65.,135.));
#9463=CARTESIAN_POINT('',(45.5,-50.,135.));
#9464=CARTESIAN_POINT('Origin',(25.5,-65.,134.));
#9465=CARTESIAN_POINT('Origin',(45.0857864376269,-65.,134.));
#9466=CARTESIAN_POINT('Origin',(49.5,-51.,60.));
#9467=CARTESIAN_POINT('',(50.5,-51.,130.));
#9468=CARTESIAN_POINT('',(50.5,-51.,40.));
#9469=CARTESIAN_POINT('',(50.5,-51.,60.));
#9470=CARTESIAN_POINT('Origin',(49.5,-51.,40.4142135623731));
#9471=CARTESIAN_POINT('Origin',(49.5,-51.,129.585786437627));
#9472=CARTESIAN_POINT('Origin',(47.2928932188134,-51.,38.2071067811866));
#9473=CARTESIAN_POINT('',(45.5,-51.,35.));
#9474=CARTESIAN_POINT('',(48.,-51.,37.5));
#9475=CARTESIAN_POINT('Origin',(45.0857864376269,-51.,36.));
#9476=CARTESIAN_POINT('Origin',(-24.5,-51.,36.));
#9477=CARTESIAN_POINT('',(-45.,-51.,35.));
#9478=CARTESIAN_POINT('',(-24.5,-51.,35.));
#9479=CARTESIAN_POINT('Origin',(-44.5857864376269,-51.,36.));
#9480=CARTESIAN_POINT('Origin',(-46.6678932188135,-51.,38.0821067811865));
#9481=CARTESIAN_POINT('',(-50.,-51.,40.));
#9482=CARTESIAN_POINT('',(-47.375,-51.,37.375));
#9483=CARTESIAN_POINT('Origin',(-49.,-51.,40.4142135623731));
#9484=CARTESIAN_POINT('Origin',(-49.,-51.,110.));
#9485=CARTESIAN_POINT('',(-50.,-51.,130.));
#9486=CARTESIAN_POINT('',(-50.,-51.,110.));
#9487=CARTESIAN_POINT('Origin',(-49.,-51.,129.585786437627));
#9488=CARTESIAN_POINT('Origin',(-46.6678932188135,-51.,131.917893218813));
#9489=CARTESIAN_POINT('',(-47.375,-51.,132.625));
#9490=CARTESIAN_POINT('Origin',(47.2928932188134,-51.,131.792893218813));
#9491=CARTESIAN_POINT('',(48.,-51.,132.5));
#9492=CARTESIAN_POINT('Origin',(-47.5,-50.,37.5));
#9493=CARTESIAN_POINT('',(-45.,-65.,35.));
#9494=CARTESIAN_POINT('',(-45.,-50.,35.));
#9495=CARTESIAN_POINT('',(-50.,-65.,40.));
#9496=CARTESIAN_POINT('',(-47.375,-65.,37.375));
#9497=CARTESIAN_POINT('',(-50.,-50.,40.));
#9498=CARTESIAN_POINT('Origin',(-49.5,-50.,35.));
#9499=CARTESIAN_POINT('',(45.5,-65.,35.));
#9500=CARTESIAN_POINT('',(45.5,-50.,35.));
#9501=CARTESIAN_POINT('',(-24.5,-65.,35.));
#9502=CARTESIAN_POINT('Origin',(48.,-50.,37.5));
#9503=CARTESIAN_POINT('',(50.5,-65.,40.));
#9504=CARTESIAN_POINT('',(50.5,-50.,40.));
#9505=CARTESIAN_POINT('',(48.,-65.,37.5));
#9506=CARTESIAN_POINT('Origin',(50.5,-50.,35.));
#9507=CARTESIAN_POINT('',(50.5,-65.,130.));
#9508=CARTESIAN_POINT('',(50.5,-50.,130.));
#9509=CARTESIAN_POINT('',(50.5,-65.,60.));
#9510=CARTESIAN_POINT('Origin',(49.5,-65.,60.));
#9511=CARTESIAN_POINT('Origin',(49.5,-65.,40.4142135623731));
#9512=CARTESIAN_POINT('Origin',(49.5,-65.,129.585786437627));
#9513=CARTESIAN_POINT('Origin',(47.2928932188134,-65.,38.2071067811866));
#9514=CARTESIAN_POINT('Origin',(45.0857864376269,-65.,36.));
#9515=CARTESIAN_POINT('Origin',(-24.5,-65.,36.));
#9516=CARTESIAN_POINT('Origin',(-44.5857864376269,-65.,36.));
#9517=CARTESIAN_POINT('Origin',(-46.6678932188135,-65.,38.0821067811865));
#9518=CARTESIAN_POINT('Origin',(-49.,-65.,40.4142135623731));
#9519=CARTESIAN_POINT('Origin',(-49.,-65.,110.));
#9520=CARTESIAN_POINT('',(-50.,-65.,130.));
#9521=CARTESIAN_POINT('',(-50.,-65.,110.));
#9522=CARTESIAN_POINT('Origin',(-49.,-65.,129.585786437627));
#9523=CARTESIAN_POINT('Origin',(-46.6678932188135,-65.,131.917893218813));
#9524=CARTESIAN_POINT('',(-45.,-65.,135.));
#9525=CARTESIAN_POINT('',(-47.375,-65.,132.625));
#9526=CARTESIAN_POINT('Origin',(-44.5857864376269,-65.,134.));
#9527=CARTESIAN_POINT('Origin',(25.5,-65.,134.));
#9528=CARTESIAN_POINT('',(25.5,-65.,135.));
#9529=CARTESIAN_POINT('Origin',(47.2928932188134,-65.,131.792893218813));
#9530=CARTESIAN_POINT('',(48.,-65.,132.5));
#9531=CARTESIAN_POINT('Origin',(-47.5,-50.,132.5));
#9532=CARTESIAN_POINT('',(-50.,-50.,130.));
#9533=CARTESIAN_POINT('',(-45.,-50.,135.));
#9534=CARTESIAN_POINT('Origin',(50.5,-50.,135.));
#9535=CARTESIAN_POINT('Origin',(48.,-50.,132.5));
#9536=CARTESIAN_POINT('Origin',(-50.,-50.,135.));
#9537=CARTESIAN_POINT('',(0.,0.,0.));
#9538=CARTESIAN_POINT('Origin',(-32.4855257306532,-32.7240321735238,86.));
#9539=CARTESIAN_POINT('',(-29.4855257306532,-32.7240321735238,62.));
#9540=CARTESIAN_POINT('Origin',(-32.4855257306532,-32.7240321735238,62.));
#9541=CARTESIAN_POINT('',(-29.4855257306532,-32.7240321735238,50.));
#9542=CARTESIAN_POINT('',(-29.4855257306532,-32.7240321735238,86.));
#9543=CARTESIAN_POINT('Origin',(-32.4855257306532,-32.7240321735238,50.));
#9544=CARTESIAN_POINT('Origin',(32.5144742693468,32.2759678264762,86.));
#9545=CARTESIAN_POINT('',(35.5144742693468,32.2759678264762,62.));
#9546=CARTESIAN_POINT('Origin',(32.5144742693468,32.2759678264762,62.));
#9547=CARTESIAN_POINT('',(35.5144742693468,32.2759678264762,50.));
#9548=CARTESIAN_POINT('',(35.5144742693468,32.2759678264762,86.));
#9549=CARTESIAN_POINT('Origin',(32.5144742693468,32.2759678264762,50.));
#9550=CARTESIAN_POINT('Origin',(-32.4855257306532,32.2759678264762,86.));
#9551=CARTESIAN_POINT('',(-29.4855257306532,32.2759678264762,62.));
#9552=CARTESIAN_POINT('Origin',(-32.4855257306532,32.2759678264762,62.));
#9553=CARTESIAN_POINT('',(-29.4855257306532,32.2759678264762,50.));
#9554=CARTESIAN_POINT('',(-29.4855257306532,32.2759678264762,86.));
#9555=CARTESIAN_POINT('Origin',(-32.4855257306532,32.2759678264762,50.));
#9556=CARTESIAN_POINT('Origin',(32.5144742693468,-7.72403217352376,86.));
#9557=CARTESIAN_POINT('',(35.5144742693468,-7.72403217352376,62.));
#9558=CARTESIAN_POINT('Origin',(32.5144742693468,-7.72403217352376,62.));
#9559=CARTESIAN_POINT('',(35.5144742693468,-7.72403217352376,50.));
#9560=CARTESIAN_POINT('',(35.5144742693468,-7.72403217352376,86.));
#9561=CARTESIAN_POINT('Origin',(32.5144742693468,-7.72403217352376,50.));
#9562=CARTESIAN_POINT('Origin',(-22.5,-49.,51.));
#9563=CARTESIAN_POINT('',(-44.5857864376269,-49.,50.));
#9564=CARTESIAN_POINT('',(15.5857864376269,-49.,50.));
#9565=CARTESIAN_POINT('',(-22.5,-49.,50.));
#9566=CARTESIAN_POINT('',(16.,-50.,51.));
#9567=CARTESIAN_POINT('Origin',(15.5857864376269,-49.,51.));
#9568=CARTESIAN_POINT('',(-45.,-50.,51.));
#9569=CARTESIAN_POINT('',(-22.5,-50.,51.));
#9570=CARTESIAN_POINT('Origin',(-44.5857864376269,-49.,51.));
#9571=CARTESIAN_POINT('Origin',(20.,-25.,51.));
#9572=CARTESIAN_POINT('',(20.,-44.5857864376269,50.));
#9573=CARTESIAN_POINT('',(20.,-30.8578643762691,50.));
#9574=CARTESIAN_POINT('',(20.,-25.,50.));
#9575=CARTESIAN_POINT('',(21.,-31.2720779386421,51.));
#9576=CARTESIAN_POINT('Origin',(20.,-30.8578643762691,51.));
#9577=CARTESIAN_POINT('',(21.,-45.,51.));
#9578=CARTESIAN_POINT('',(21.,-25.,51.));
#9579=CARTESIAN_POINT('Origin',(20.,-44.5857864376269,51.));
#9580=CARTESIAN_POINT('Origin',(22.860912703474,-27.9969516727951,51.));
#9581=CARTESIAN_POINT('',(30.857864376269,-20.,50.));
#9582=CARTESIAN_POINT('',(22.860912703474,-27.9969516727951,50.));
#9583=CARTESIAN_POINT('',(31.2720779386421,-21.,51.));
#9584=CARTESIAN_POINT('Origin',(30.857864376269,-20.,51.));
#9585=CARTESIAN_POINT('',(23.5680194846605,-28.7040584539816,51.));
#9586=CARTESIAN_POINT('Origin',(49.,-10.5,51.));
#9587=CARTESIAN_POINT('',(50.,45.,51.));
#9588=CARTESIAN_POINT('',(50.,-16.,51.));
#9589=CARTESIAN_POINT('',(50.,-10.5,51.));
#9590=CARTESIAN_POINT('',(49.,-15.5857864376269,50.));
#9591=CARTESIAN_POINT('Origin',(49.,-15.5857864376269,51.));
#9592=CARTESIAN_POINT('',(49.,44.5857864376269,50.));
#9593=CARTESIAN_POINT('',(49.,-10.5,50.));
#9594=CARTESIAN_POINT('Origin',(49.,44.5857864376269,51.));
#9595=CARTESIAN_POINT('Origin',(15.6360389693211,-20.,51.));
#9596=CARTESIAN_POINT('',(44.5857864376269,-20.,50.));
#9597=CARTESIAN_POINT('',(15.6360389693211,-20.,50.));
#9598=CARTESIAN_POINT('',(45.,-21.,51.));
#9599=CARTESIAN_POINT('Origin',(44.5857864376269,-20.,51.));
#9600=CARTESIAN_POINT('',(15.6360389693211,-21.,51.));
#9601=CARTESIAN_POINT('Origin',(39.5428932188134,-25.0428932188135,51.));
#9602=CARTESIAN_POINT('',(40.25,-25.75,51.));
#9603=CARTESIAN_POINT('',(39.5428932188134,-25.0428932188135,50.));
#9604=CARTESIAN_POINT('Origin',(48.0428932188135,45.5428932188135,51.));
#9605=CARTESIAN_POINT('',(45.,50.,51.));
#9606=CARTESIAN_POINT('',(48.75,46.25,51.));
#9607=CARTESIAN_POINT('',(44.5857864376269,49.,50.));
#9608=CARTESIAN_POINT('',(48.0428932188135,45.5428932188135,50.));
#9609=CARTESIAN_POINT('Origin',(44.5857864376269,49.,51.));
#9610=CARTESIAN_POINT('Origin',(22.5,49.,51.));
#9611=CARTESIAN_POINT('',(-45.,50.,51.));
#9612=CARTESIAN_POINT('',(22.5,50.,51.));
#9613=CARTESIAN_POINT('',(-44.5857864376269,49.,50.));
#9614=CARTESIAN_POINT('',(22.5,49.,50.));
#9615=CARTESIAN_POINT('Origin',(-44.5857864376269,49.,51.));
#9616=CARTESIAN_POINT('Origin',(25.0428932188134,-39.5428932188134,51.));
#9617=CARTESIAN_POINT('',(25.0428932188134,-39.5428932188134,50.));
#9618=CARTESIAN_POINT('',(25.75,-40.25,51.));
#9619=CARTESIAN_POINT('Origin',(-45.5428932188135,48.0428932188135,51.));
#9620=CARTESIAN_POINT('',(-50.,45.,51.));
#9621=CARTESIAN_POINT('',(-46.25,48.75,51.));
#9622=CARTESIAN_POINT('',(-49.,44.5857864376269,50.));
#9623=CARTESIAN_POINT('',(-45.5428932188135,48.0428932188135,50.));
#9624=CARTESIAN_POINT('Origin',(-49.,44.5857864376269,51.));
#9625=CARTESIAN_POINT('Origin',(-49.,22.5,51.));
#9626=CARTESIAN_POINT('',(-50.,-45.,51.));
#9627=CARTESIAN_POINT('',(-50.,22.5,51.));
#9628=CARTESIAN_POINT('',(-49.,-44.5857864376269,50.));
#9629=CARTESIAN_POINT('',(-49.,22.5,50.));
#9630=CARTESIAN_POINT('Origin',(-49.,-44.5857864376269,51.));
#9631=CARTESIAN_POINT('Origin',(-48.0428932188135,-45.5428932188135,51.));
#9632=CARTESIAN_POINT('',(-48.75,-46.25,51.));
#9633=CARTESIAN_POINT('',(-48.0428932188135,-45.5428932188135,50.));
#9634=CARTESIAN_POINT('Origin',(18.5,-47.5,50.));
#9635=CARTESIAN_POINT('',(21.,-45.,61.));
#9636=CARTESIAN_POINT('',(21.,-45.,50.));
#9637=CARTESIAN_POINT('',(16.,-50.,61.));
#9638=CARTESIAN_POINT('',(25.75,-40.25,61.));
#9639=CARTESIAN_POINT('',(16.,-50.,50.));
#9640=CARTESIAN_POINT('Origin',(21.,-50.,50.));
#9641=CARTESIAN_POINT('',(21.,-31.2720779386421,61.));
#9642=CARTESIAN_POINT('',(21.,-31.2720779386421,50.));
#9643=CARTESIAN_POINT('',(21.,-25.,61.));
#9644=CARTESIAN_POINT('Origin',(21.,-31.2720779386421,50.));
#9645=CARTESIAN_POINT('',(31.2720779386421,-21.,61.));
#9646=CARTESIAN_POINT('',(31.2720779386421,-21.,50.));
#9647=CARTESIAN_POINT('',(23.5680194846605,-28.7040584539816,61.));
#9648=CARTESIAN_POINT('Origin',(31.2720779386421,-21.,50.));
#9649=CARTESIAN_POINT('',(45.,-21.,61.));
#9650=CARTESIAN_POINT('',(45.,-21.,50.));
#9651=CARTESIAN_POINT('',(15.6360389693211,-21.,61.));
#9652=CARTESIAN_POINT('Origin',(47.5,-18.5,50.));
#9653=CARTESIAN_POINT('',(50.,-16.,61.));
#9654=CARTESIAN_POINT('',(50.,-16.,50.));
#9655=CARTESIAN_POINT('',(40.25,-25.75,61.));
#9656=CARTESIAN_POINT('Origin',(50.,-21.,50.));
#9657=CARTESIAN_POINT('',(50.,45.,61.));
#9658=CARTESIAN_POINT('',(50.,45.,50.));
#9659=CARTESIAN_POINT('',(50.,-10.5,61.));
#9660=CARTESIAN_POINT('Origin',(0.,0.,50.));
#9661=CARTESIAN_POINT('Origin',(-48.0428932188135,-45.5428932188135,61.));
#9662=CARTESIAN_POINT('',(-44.5857864376269,-49.,62.));
#9663=CARTESIAN_POINT('',(-49.,-44.5857864376269,62.));
#9664=CARTESIAN_POINT('',(-48.0428932188135,-45.5428932188135,62.));
#9665=CARTESIAN_POINT('',(-50.,-45.,61.));
#9666=CARTESIAN_POINT('Origin',(-49.,-44.5857864376269,61.));
#9667=CARTESIAN_POINT('',(-45.,-50.,61.));
#9668=CARTESIAN_POINT('',(-48.75,-46.25,61.));
#9669=CARTESIAN_POINT('Origin',(-44.5857864376269,-49.,61.));
#9670=CARTESIAN_POINT('Origin',(-49.,22.5,61.));
#9671=CARTESIAN_POINT('',(-49.,44.5857864376269,62.));
#9672=CARTESIAN_POINT('',(-49.,22.5,62.));
#9673=CARTESIAN_POINT('',(-50.,45.,61.));
#9674=CARTESIAN_POINT('Origin',(-49.,44.5857864376269,61.));
#9675=CARTESIAN_POINT('',(-50.,22.5,61.));
#9676=CARTESIAN_POINT('Origin',(-45.5428932188135,48.0428932188135,61.));
#9677=CARTESIAN_POINT('',(-44.5857864376269,49.,62.));
#9678=CARTESIAN_POINT('',(-45.5428932188135,48.0428932188135,62.));
#9679=CARTESIAN_POINT('',(-45.,50.,61.));
#9680=CARTESIAN_POINT('Origin',(-44.5857864376269,49.,61.));
#9681=CARTESIAN_POINT('',(-46.25,48.75,61.));
#9682=CARTESIAN_POINT('Origin',(22.5,49.,61.));
#9683=CARTESIAN_POINT('',(44.5857864376269,49.,62.));
#9684=CARTESIAN_POINT('',(22.5,49.,62.));
#9685=CARTESIAN_POINT('',(45.,50.,61.));
#9686=CARTESIAN_POINT('Origin',(44.5857864376269,49.,61.));
#9687=CARTESIAN_POINT('',(22.5,50.,61.));
#9688=CARTESIAN_POINT('Origin',(48.0428932188135,45.5428932188135,61.));
#9689=CARTESIAN_POINT('',(49.,44.5857864376269,62.));
#9690=CARTESIAN_POINT('',(48.0428932188135,45.5428932188135,62.));
#9691=CARTESIAN_POINT('Origin',(49.,44.5857864376269,61.));
#9692=CARTESIAN_POINT('',(48.75,46.25,61.));
#9693=CARTESIAN_POINT('Origin',(49.,-10.5,61.));
#9694=CARTESIAN_POINT('',(49.,-15.5857864376269,62.));
#9695=CARTESIAN_POINT('',(49.,-10.5,62.));
#9696=CARTESIAN_POINT('Origin',(49.,-15.5857864376269,61.));
#9697=CARTESIAN_POINT('Origin',(39.5428932188134,-25.0428932188135,61.));
#9698=CARTESIAN_POINT('',(44.5857864376269,-20.,62.));
#9699=CARTESIAN_POINT('',(39.5428932188134,-25.0428932188135,62.));
#9700=CARTESIAN_POINT('Origin',(44.5857864376269,-20.,61.));
#9701=CARTESIAN_POINT('Origin',(15.6360389693211,-20.,61.));
#9702=CARTESIAN_POINT('',(30.857864376269,-20.,62.));
#9703=CARTESIAN_POINT('',(15.6360389693211,-20.,62.));
#9704=CARTESIAN_POINT('Origin',(30.857864376269,-20.,61.));
#9705=CARTESIAN_POINT('Origin',(22.860912703474,-27.9969516727951,61.));
#9706=CARTESIAN_POINT('',(20.,-30.8578643762691,62.));
#9707=CARTESIAN_POINT('',(22.860912703474,-27.9969516727951,62.));
#9708=CARTESIAN_POINT('Origin',(20.,-30.8578643762691,61.));
#9709=CARTESIAN_POINT('Origin',(20.,-25.,61.));
#9710=CARTESIAN_POINT('',(20.,-44.5857864376269,62.));
#9711=CARTESIAN_POINT('',(20.,-25.,62.));
#9712=CARTESIAN_POINT('Origin',(20.,-44.5857864376269,61.));
#9713=CARTESIAN_POINT('Origin',(25.0428932188134,-39.5428932188134,61.));
#9714=CARTESIAN_POINT('',(15.5857864376269,-49.,62.));
#9715=CARTESIAN_POINT('',(25.0428932188134,-39.5428932188134,62.));
#9716=CARTESIAN_POINT('Origin',(15.5857864376269,-49.,61.));
#9717=CARTESIAN_POINT('Origin',(-22.5,-49.,61.));
#9718=CARTESIAN_POINT('',(-22.5,-50.,61.));
#9719=CARTESIAN_POINT('',(-22.5,-49.,62.));
#9720=CARTESIAN_POINT('Origin',(-45.,-50.,50.));
#9721=CARTESIAN_POINT('',(-45.,-50.,50.));
#9722=CARTESIAN_POINT('Origin',(-50.,-45.,50.));
#9723=CARTESIAN_POINT('',(-50.,-45.,50.));
#9724=CARTESIAN_POINT('Origin',(0.,0.,62.));
#9725=CARTESIAN_POINT('Origin',(-50.,45.,50.));
#9726=CARTESIAN_POINT('',(-50.,45.,50.));
#9727=CARTESIAN_POINT('Origin',(-45.,50.,50.));
#9728=CARTESIAN_POINT('',(-45.,50.,50.));
#9729=CARTESIAN_POINT('Origin',(45.,50.,50.));
#9730=CARTESIAN_POINT('',(45.,50.,50.));
#9731=CARTESIAN_POINT('Origin',(50.,45.,50.));
#9732=CARTESIAN_POINT('',(0.,0.,0.));
#9733=CARTESIAN_POINT('Origin',(-32.4855257306532,-32.7240321735238,86.));
#9734=CARTESIAN_POINT('',(-29.4855257306532,-32.7240321735238,74.));
#9735=CARTESIAN_POINT('Origin',(-32.4855257306532,-32.7240321735238,74.));
#9736=CARTESIAN_POINT('',(-29.4855257306532,-32.7240321735238,62.));
#9737=CARTESIAN_POINT('',(-29.4855257306532,-32.7240321735238,86.));
#9738=CARTESIAN_POINT('Origin',(-32.4855257306532,-32.7240321735238,62.));
#9739=CARTESIAN_POINT('Origin',(32.5144742693468,32.2759678264762,86.));
#9740=CARTESIAN_POINT('',(35.5144742693468,32.2759678264762,74.));
#9741=CARTESIAN_POINT('Origin',(32.5144742693468,32.2759678264762,74.));
#9742=CARTESIAN_POINT('',(35.5144742693468,32.2759678264762,62.));
#9743=CARTESIAN_POINT('',(35.5144742693468,32.2759678264762,86.));
#9744=CARTESIAN_POINT('Origin',(32.5144742693468,32.2759678264762,62.));
#9745=CARTESIAN_POINT('Origin',(-32.4855257306532,32.2759678264762,86.));
#9746=CARTESIAN_POINT('',(-29.4855257306532,32.2759678264762,74.));
#9747=CARTESIAN_POINT('Origin',(-32.4855257306532,32.2759678264762,74.));
#9748=CARTESIAN_POINT('',(-29.4855257306532,32.2759678264762,62.));
#9749=CARTESIAN_POINT('',(-29.4855257306532,32.2759678264762,86.));
#9750=CARTESIAN_POINT('Origin',(-32.4855257306532,32.2759678264762,62.));
#9751=CARTESIAN_POINT('Origin',(32.5144742693468,-7.72403217352376,86.));
#9752=CARTESIAN_POINT('',(35.5144742693468,-7.72403217352376,74.));
#9753=CARTESIAN_POINT('Origin',(32.5144742693468,-7.72403217352376,74.));
#9754=CARTESIAN_POINT('',(35.5144742693468,-7.72403217352376,62.));
#9755=CARTESIAN_POINT('',(35.5144742693468,-7.72403217352376,86.));
#9756=CARTESIAN_POINT('Origin',(32.5144742693468,-7.72403217352376,62.));
#9757=CARTESIAN_POINT('Origin',(-22.5,-49.,63.));
#9758=CARTESIAN_POINT('',(-44.5857864376269,-49.,62.));
#9759=CARTESIAN_POINT('',(15.5857864376269,-49.,62.));
#9760=CARTESIAN_POINT('',(-22.5,-49.,62.));
#9761=CARTESIAN_POINT('',(16.,-50.,63.));
#9762=CARTESIAN_POINT('Origin',(15.5857864376269,-49.,63.));
#9763=CARTESIAN_POINT('',(-45.,-50.,63.));
#9764=CARTESIAN_POINT('',(-22.5,-50.,63.));
#9765=CARTESIAN_POINT('Origin',(-44.5857864376269,-49.,63.));
#9766=CARTESIAN_POINT('Origin',(20.,-25.,63.));
#9767=CARTESIAN_POINT('',(20.,-44.5857864376269,62.));
#9768=CARTESIAN_POINT('',(20.,-30.8578643762691,62.));
#9769=CARTESIAN_POINT('',(20.,-25.,62.));
#9770=CARTESIAN_POINT('',(21.,-31.2720779386421,63.));
#9771=CARTESIAN_POINT('Origin',(20.,-30.8578643762691,63.));
#9772=CARTESIAN_POINT('',(21.,-45.,63.));
#9773=CARTESIAN_POINT('',(21.,-25.,63.));
#9774=CARTESIAN_POINT('Origin',(20.,-44.5857864376269,63.));
#9775=CARTESIAN_POINT('Origin',(22.860912703474,-27.9969516727951,63.));
#9776=CARTESIAN_POINT('',(30.857864376269,-20.,62.));
#9777=CARTESIAN_POINT('',(22.860912703474,-27.9969516727951,62.));
#9778=CARTESIAN_POINT('',(31.2720779386421,-21.,63.));
#9779=CARTESIAN_POINT('Origin',(30.857864376269,-20.,63.));
#9780=CARTESIAN_POINT('',(23.5680194846605,-28.7040584539816,63.));
#9781=CARTESIAN_POINT('Origin',(49.,-10.5,63.));
#9782=CARTESIAN_POINT('',(50.,45.,63.));
#9783=CARTESIAN_POINT('',(50.,-16.,63.));
#9784=CARTESIAN_POINT('',(50.,-10.5,63.));
#9785=CARTESIAN_POINT('',(49.,-15.5857864376269,62.));
#9786=CARTESIAN_POINT('Origin',(49.,-15.5857864376269,63.));
#9787=CARTESIAN_POINT('',(49.,44.5857864376269,62.));
#9788=CARTESIAN_POINT('',(49.,-10.5,62.));
#9789=CARTESIAN_POINT('Origin',(49.,44.5857864376269,63.));
#9790=CARTESIAN_POINT('Origin',(15.6360389693211,-20.,63.));
#9791=CARTESIAN_POINT('',(44.5857864376269,-20.,62.));
#9792=CARTESIAN_POINT('',(15.6360389693211,-20.,62.));
#9793=CARTESIAN_POINT('',(45.,-21.,63.));
#9794=CARTESIAN_POINT('Origin',(44.5857864376269,-20.,63.));
#9795=CARTESIAN_POINT('',(15.6360389693211,-21.,63.));
#9796=CARTESIAN_POINT('Origin',(39.5428932188134,-25.0428932188135,63.));
#9797=CARTESIAN_POINT('',(40.25,-25.75,63.));
#9798=CARTESIAN_POINT('',(39.5428932188134,-25.0428932188135,62.));
#9799=CARTESIAN_POINT('Origin',(48.0428932188135,45.5428932188135,63.));
#9800=CARTESIAN_POINT('',(45.,50.,63.));
#9801=CARTESIAN_POINT('',(48.75,46.25,63.));
#9802=CARTESIAN_POINT('',(44.5857864376269,49.,62.));
#9803=CARTESIAN_POINT('',(48.0428932188135,45.5428932188135,62.));
#9804=CARTESIAN_POINT('Origin',(44.5857864376269,49.,63.));
#9805=CARTESIAN_POINT('Origin',(22.5,49.,63.));
#9806=CARTESIAN_POINT('',(-45.,50.,63.));
#9807=CARTESIAN_POINT('',(22.5,50.,63.));
#9808=CARTESIAN_POINT('',(-44.5857864376269,49.,62.));
#9809=CARTESIAN_POINT('',(22.5,49.,62.));
#9810=CARTESIAN_POINT('Origin',(-44.5857864376269,49.,63.));
#9811=CARTESIAN_POINT('Origin',(25.0428932188134,-39.5428932188134,63.));
#9812=CARTESIAN_POINT('',(25.0428932188134,-39.5428932188134,62.));
#9813=CARTESIAN_POINT('',(25.75,-40.25,63.));
#9814=CARTESIAN_POINT('Origin',(-45.5428932188135,48.0428932188135,63.));
#9815=CARTESIAN_POINT('',(-50.,45.,63.));
#9816=CARTESIAN_POINT('',(-46.25,48.75,63.));
#9817=CARTESIAN_POINT('',(-49.,44.5857864376269,62.));
#9818=CARTESIAN_POINT('',(-45.5428932188135,48.0428932188135,62.));
#9819=CARTESIAN_POINT('Origin',(-49.,44.5857864376269,63.));
#9820=CARTESIAN_POINT('Origin',(-49.,22.5,63.));
#9821=CARTESIAN_POINT('',(-50.,-45.,63.));
#9822=CARTESIAN_POINT('',(-50.,22.5,63.));
#9823=CARTESIAN_POINT('',(-49.,-44.5857864376269,62.));
#9824=CARTESIAN_POINT('',(-49.,22.5,62.));
#9825=CARTESIAN_POINT('Origin',(-49.,-44.5857864376269,63.));
#9826=CARTESIAN_POINT('Origin',(-48.0428932188135,-45.5428932188135,63.));
#9827=CARTESIAN_POINT('',(-48.75,-46.25,63.));
#9828=CARTESIAN_POINT('',(-48.0428932188135,-45.5428932188135,62.));
#9829=CARTESIAN_POINT('Origin',(18.5,-47.5,62.));
#9830=CARTESIAN_POINT('',(21.,-45.,73.));
#9831=CARTESIAN_POINT('',(21.,-45.,62.));
#9832=CARTESIAN_POINT('',(16.,-50.,73.));
#9833=CARTESIAN_POINT('',(25.75,-40.25,73.));
#9834=CARTESIAN_POINT('',(16.,-50.,62.));
#9835=CARTESIAN_POINT('Origin',(21.,-50.,62.));
#9836=CARTESIAN_POINT('',(21.,-31.2720779386421,73.));
#9837=CARTESIAN_POINT('',(21.,-31.2720779386421,62.));
#9838=CARTESIAN_POINT('',(21.,-25.,73.));
#9839=CARTESIAN_POINT('Origin',(21.,-31.2720779386421,62.));
#9840=CARTESIAN_POINT('',(31.2720779386421,-21.,73.));
#9841=CARTESIAN_POINT('',(31.2720779386421,-21.,62.));
#9842=CARTESIAN_POINT('',(23.5680194846605,-28.7040584539816,73.));
#9843=CARTESIAN_POINT('Origin',(31.2720779386421,-21.,62.));
#9844=CARTESIAN_POINT('',(45.,-21.,73.));
#9845=CARTESIAN_POINT('',(45.,-21.,62.));
#9846=CARTESIAN_POINT('',(15.6360389693211,-21.,73.));
#9847=CARTESIAN_POINT('Origin',(47.5,-18.5,62.));
#9848=CARTESIAN_POINT('',(50.,-16.,73.));
#9849=CARTESIAN_POINT('',(50.,-16.,62.));
#9850=CARTESIAN_POINT('',(40.25,-25.75,73.));
#9851=CARTESIAN_POINT('Origin',(50.,-21.,62.));
#9852=CARTESIAN_POINT('',(50.,45.,73.));
#9853=CARTESIAN_POINT('',(50.,45.,62.));
#9854=CARTESIAN_POINT('',(50.,-10.5,73.));
#9855=CARTESIAN_POINT('Origin',(0.,0.,62.));
#9856=CARTESIAN_POINT('Origin',(-48.0428932188135,-45.5428932188135,73.));
#9857=CARTESIAN_POINT('',(-44.5857864376269,-49.,74.));
#9858=CARTESIAN_POINT('',(-49.,-44.5857864376269,74.));
#9859=CARTESIAN_POINT('',(-48.0428932188135,-45.5428932188135,74.));
#9860=CARTESIAN_POINT('',(-50.,-45.,73.));
#9861=CARTESIAN_POINT('Origin',(-49.,-44.5857864376269,73.));
#9862=CARTESIAN_POINT('',(-45.,-50.,73.));
#9863=CARTESIAN_POINT('',(-48.75,-46.25,73.));
#9864=CARTESIAN_POINT('Origin',(-44.5857864376269,-49.,73.));
#9865=CARTESIAN_POINT('Origin',(-49.,22.5,73.));
#9866=CARTESIAN_POINT('',(-49.,44.5857864376269,74.));
#9867=CARTESIAN_POINT('',(-49.,22.5,74.));
#9868=CARTESIAN_POINT('',(-50.,45.,73.));
#9869=CARTESIAN_POINT('Origin',(-49.,44.5857864376269,73.));
#9870=CARTESIAN_POINT('',(-50.,22.5,73.));
#9871=CARTESIAN_POINT('Origin',(-45.5428932188135,48.0428932188135,73.));
#9872=CARTESIAN_POINT('',(-44.5857864376269,49.,74.));
#9873=CARTESIAN_POINT('',(-45.5428932188135,48.0428932188135,74.));
#9874=CARTESIAN_POINT('',(-45.,50.,73.));
#9875=CARTESIAN_POINT('Origin',(-44.5857864376269,49.,73.));
#9876=CARTESIAN_POINT('',(-46.25,48.75,73.));
#9877=CARTESIAN_POINT('Origin',(22.5,49.,73.));
#9878=CARTESIAN_POINT('',(44.5857864376269,49.,74.));
#9879=CARTESIAN_POINT('',(22.5,49.,74.));
#9880=CARTESIAN_POINT('',(45.,50.,73.));
#9881=CARTESIAN_POINT('Origin',(44.5857864376269,49.,73.));
#9882=CARTESIAN_POINT('',(22.5,50.,73.));
#9883=CARTESIAN_POINT('Origin',(48.0428932188135,45.5428932188135,73.));
#9884=CARTESIAN_POINT('',(49.,44.5857864376269,74.));
#9885=CARTESIAN_POINT('',(48.0428932188135,45.5428932188135,74.));
#9886=CARTESIAN_POINT('Origin',(49.,44.5857864376269,73.));
#9887=CARTESIAN_POINT('',(48.75,46.25,73.));
#9888=CARTESIAN_POINT('Origin',(49.,-10.5,73.));
#9889=CARTESIAN_POINT('',(49.,-15.5857864376269,74.));
#9890=CARTESIAN_POINT('',(49.,-10.5,74.));
#9891=CARTESIAN_POINT('Origin',(49.,-15.5857864376269,73.));
#9892=CARTESIAN_POINT('Origin',(39.5428932188134,-25.0428932188135,73.));
#9893=CARTESIAN_POINT('',(44.5857864376269,-20.,74.));
#9894=CARTESIAN_POINT('',(39.5428932188134,-25.0428932188135,74.));
#9895=CARTESIAN_POINT('Origin',(44.5857864376269,-20.,73.));
#9896=CARTESIAN_POINT('Origin',(15.6360389693211,-20.,73.));
#9897=CARTESIAN_POINT('',(30.857864376269,-20.,74.));
#9898=CARTESIAN_POINT('',(15.6360389693211,-20.,74.));
#9899=CARTESIAN_POINT('Origin',(30.857864376269,-20.,73.));
#9900=CARTESIAN_POINT('Origin',(22.860912703474,-27.9969516727951,73.));
#9901=CARTESIAN_POINT('',(20.,-30.8578643762691,74.));
#9902=CARTESIAN_POINT('',(22.860912703474,-27.9969516727951,74.));
#9903=CARTESIAN_POINT('Origin',(20.,-30.8578643762691,73.));
#9904=CARTESIAN_POINT('Origin',(20.,-25.,73.));
#9905=CARTESIAN_POINT('',(20.,-44.5857864376269,74.));
#9906=CARTESIAN_POINT('',(20.,-25.,74.));
#9907=CARTESIAN_POINT('Origin',(20.,-44.5857864376269,73.));
#9908=CARTESIAN_POINT('Origin',(25.0428932188134,-39.5428932188134,73.));
#9909=CARTESIAN_POINT('',(15.5857864376269,-49.,74.));
#9910=CARTESIAN_POINT('',(25.0428932188134,-39.5428932188134,74.));
#9911=CARTESIAN_POINT('Origin',(15.5857864376269,-49.,73.));
#9912=CARTESIAN_POINT('Origin',(-22.5,-49.,73.));
#9913=CARTESIAN_POINT('',(-22.5,-50.,73.));
#9914=CARTESIAN_POINT('',(-22.5,-49.,74.));
#9915=CARTESIAN_POINT('Origin',(-45.,-50.,62.));
#9916=CARTESIAN_POINT('',(-45.,-50.,62.));
#9917=CARTESIAN_POINT('Origin',(-50.,-45.,62.));
#9918=CARTESIAN_POINT('',(-50.,-45.,62.));
#9919=CARTESIAN_POINT('Origin',(0.,0.,74.));
#9920=CARTESIAN_POINT('Origin',(-50.,45.,62.));
#9921=CARTESIAN_POINT('',(-50.,45.,62.));
#9922=CARTESIAN_POINT('Origin',(-45.,50.,62.));
#9923=CARTESIAN_POINT('',(-45.,50.,62.));
#9924=CARTESIAN_POINT('Origin',(45.,50.,62.));
#9925=CARTESIAN_POINT('',(45.,50.,62.));
#9926=CARTESIAN_POINT('Origin',(50.,45.,62.));
#9927=CARTESIAN_POINT('',(0.,0.,0.));
#9928=CARTESIAN_POINT('Origin',(29.,-25.,36.));
#9929=CARTESIAN_POINT('',(30.,-35.,36.));
#9930=CARTESIAN_POINT('',(30.,-45.,36.));
#9931=CARTESIAN_POINT('',(30.,-25.,36.));
#9932=CARTESIAN_POINT('',(29.,-44.5857864376269,35.));
#9933=CARTESIAN_POINT('Origin',(29.,-44.5857864376269,36.));
#9934=CARTESIAN_POINT('',(29.,-34.5857864376269,35.));
#9935=CARTESIAN_POINT('',(29.,-25.,35.));
#9936=CARTESIAN_POINT('Origin',(29.,-34.5857864376269,36.));
#9937=CARTESIAN_POINT('Origin',(15.,-29.,36.));
#9938=CARTESIAN_POINT('',(34.5857864376269,-29.,35.));
#9939=CARTESIAN_POINT('',(44.5857864376269,-29.,35.));
#9940=CARTESIAN_POINT('',(15.,-29.,35.));
#9941=CARTESIAN_POINT('',(45.,-30.,36.));
#9942=CARTESIAN_POINT('Origin',(44.5857864376269,-29.,36.));
#9943=CARTESIAN_POINT('',(35.,-30.,36.));
#9944=CARTESIAN_POINT('',(15.,-30.,36.));
#9945=CARTESIAN_POINT('Origin',(34.5857864376269,-29.,36.));
#9946=CARTESIAN_POINT('Origin',(41.7928932188135,-31.7928932188135,36.));
#9947=CARTESIAN_POINT('',(49.,-24.5857864376269,35.));
#9948=CARTESIAN_POINT('',(41.7928932188135,-31.7928932188135,35.));
#9949=CARTESIAN_POINT('',(50.,-25.,36.));
#9950=CARTESIAN_POINT('Origin',(49.,-24.5857864376269,36.));
#9951=CARTESIAN_POINT('',(42.5,-32.5,36.));
#9952=CARTESIAN_POINT('Origin',(49.,-15.,36.));
#9953=CARTESIAN_POINT('',(49.,44.5857864376269,35.));
#9954=CARTESIAN_POINT('',(49.,-15.,35.));
#9955=CARTESIAN_POINT('',(50.,45.,36.));
#9956=CARTESIAN_POINT('Origin',(49.,44.5857864376269,36.));
#9957=CARTESIAN_POINT('',(50.,-15.,36.));
#9958=CARTESIAN_POINT('Origin',(46.7928932188135,46.7928932188135,36.));
#9959=CARTESIAN_POINT('',(44.5857864376269,49.,35.));
#9960=CARTESIAN_POINT('',(46.7928932188135,46.7928932188135,35.));
#9961=CARTESIAN_POINT('',(45.,50.,36.));
#9962=CARTESIAN_POINT('Origin',(44.5857864376269,49.,36.));
#9963=CARTESIAN_POINT('',(47.5,47.5,36.));
#9964=CARTESIAN_POINT('Origin',(25.,49.,36.));
#9965=CARTESIAN_POINT('',(-44.5857864376269,49.,35.));
#9966=CARTESIAN_POINT('',(25.,49.,35.));
#9967=CARTESIAN_POINT('',(-45.,50.,36.));
#9968=CARTESIAN_POINT('Origin',(-44.5857864376269,49.,36.));
#9969=CARTESIAN_POINT('',(25.,50.,36.));
#9970=CARTESIAN_POINT('Origin',(-46.7928932188135,46.7928932188135,36.));
#9971=CARTESIAN_POINT('',(-50.,45.,36.));
#9972=CARTESIAN_POINT('',(-47.5,47.5,36.));
#9973=CARTESIAN_POINT('',(-49.,44.5857864376269,35.));
#9974=CARTESIAN_POINT('',(-46.7928932188135,46.7928932188135,35.));
#9975=CARTESIAN_POINT('Origin',(-49.,44.5857864376269,36.));
#9976=CARTESIAN_POINT('Origin',(-49.,25.,36.));
#9977=CARTESIAN_POINT('',(-50.,-45.,36.));
#9978=CARTESIAN_POINT('',(-50.,25.,36.));
#9979=CARTESIAN_POINT('',(-49.,-44.5857864376269,35.));
#9980=CARTESIAN_POINT('',(-49.,25.,35.));
#9981=CARTESIAN_POINT('Origin',(-49.,-44.5857864376269,36.));
#9982=CARTESIAN_POINT('Origin',(-46.7928932188135,-46.7928932188135,36.));
#9983=CARTESIAN_POINT('',(-45.,-50.,36.));
#9984=CARTESIAN_POINT('',(-47.5,-47.5,36.));
#9985=CARTESIAN_POINT('',(-44.5857864376269,-49.,35.));
#9986=CARTESIAN_POINT('',(-46.7928932188135,-46.7928932188135,35.));
#9987=CARTESIAN_POINT('Origin',(-44.5857864376269,-49.,36.));
#9988=CARTESIAN_POINT('Origin',(-25.,-49.,36.));
#9989=CARTESIAN_POINT('',(25.,-50.,36.));
#9990=CARTESIAN_POINT('',(-25.,-50.,36.));
#9991=CARTESIAN_POINT('',(24.5857864376269,-49.,35.));
#9992=CARTESIAN_POINT('',(-25.,-49.,35.));
#9993=CARTESIAN_POINT('Origin',(24.5857864376269,-49.,36.));
#9994=CARTESIAN_POINT('Origin',(31.7928932188135,-41.7928932188135,36.));
#9995=CARTESIAN_POINT('',(32.5,-42.5,36.));
#9996=CARTESIAN_POINT('',(31.7928932188135,-41.7928932188135,35.));
#9997=CARTESIAN_POINT('Origin',(31.7928932188135,-31.7928932188135,36.));
#9998=CARTESIAN_POINT('',(32.5,-32.5,36.));
#9999=CARTESIAN_POINT('',(31.7928932188135,-31.7928932188135,35.));
#10000=CARTESIAN_POINT('Origin',(-47.5,-47.5,35.));
#10001=CARTESIAN_POINT('',(-45.,-50.,49.));
#10002=CARTESIAN_POINT('',(-45.,-50.,35.));
#10003=CARTESIAN_POINT('',(-50.,-45.,49.));
#10004=CARTESIAN_POINT('',(-47.5,-47.5,49.));
#10005=CARTESIAN_POINT('',(-50.,-45.,35.));
#10006=CARTESIAN_POINT('Origin',(-50.,-50.,35.));
#10007=CARTESIAN_POINT('',(25.,-50.,49.));
#10008=CARTESIAN_POINT('',(25.,-50.,35.));
#10009=CARTESIAN_POINT('',(-25.,-50.,49.));
#10010=CARTESIAN_POINT('Origin',(27.5,-47.5,35.));
#10011=CARTESIAN_POINT('',(30.,-45.,49.));
#10012=CARTESIAN_POINT('',(30.,-45.,35.));
#10013=CARTESIAN_POINT('',(32.5,-42.5,49.));
#10014=CARTESIAN_POINT('Origin',(30.,-50.,35.));
#10015=CARTESIAN_POINT('',(30.,-35.,49.));
#10016=CARTESIAN_POINT('',(30.,-35.,35.));
#10017=CARTESIAN_POINT('',(30.,-25.,49.));
#10018=CARTESIAN_POINT('Origin',(32.5,-32.5,35.));
#10019=CARTESIAN_POINT('',(35.,-30.,49.));
#10020=CARTESIAN_POINT('',(35.,-30.,35.));
#10021=CARTESIAN_POINT('',(32.5,-32.5,49.));
#10022=CARTESIAN_POINT('Origin',(30.,-30.,35.));
#10023=CARTESIAN_POINT('',(45.,-30.,49.));
#10024=CARTESIAN_POINT('',(45.,-30.,35.));
#10025=CARTESIAN_POINT('',(15.,-30.,49.));
#10026=CARTESIAN_POINT('Origin',(0.,0.,35.));
#10027=CARTESIAN_POINT('Origin',(29.,-25.,49.));
#10028=CARTESIAN_POINT('',(29.,-34.5857864376269,50.));
#10029=CARTESIAN_POINT('',(29.,-44.5857864376269,50.));
#10030=CARTESIAN_POINT('',(29.,-25.,50.));
#10031=CARTESIAN_POINT('Origin',(29.,-44.5857864376269,49.));
#10032=CARTESIAN_POINT('Origin',(29.,-34.5857864376269,49.));
#10033=CARTESIAN_POINT('Origin',(31.7928932188135,-41.7928932188135,49.));
#10034=CARTESIAN_POINT('',(24.5857864376269,-49.,50.));
#10035=CARTESIAN_POINT('',(31.7928932188135,-41.7928932188135,50.));
#10036=CARTESIAN_POINT('Origin',(24.5857864376269,-49.,49.));
#10037=CARTESIAN_POINT('Origin',(-25.,-49.,49.));
#10038=CARTESIAN_POINT('',(-44.5857864376269,-49.,50.));
#10039=CARTESIAN_POINT('',(-25.,-49.,50.));
#10040=CARTESIAN_POINT('Origin',(-44.5857864376269,-49.,49.));
#10041=CARTESIAN_POINT('Origin',(-46.7928932188135,-46.7928932188135,49.));
#10042=CARTESIAN_POINT('',(-49.,-44.5857864376269,50.));
#10043=CARTESIAN_POINT('',(-46.7928932188135,-46.7928932188135,50.));
#10044=CARTESIAN_POINT('Origin',(-49.,-44.5857864376269,49.));
#10045=CARTESIAN_POINT('Origin',(-49.,25.,49.));
#10046=CARTESIAN_POINT('',(-49.,44.5857864376269,50.));
#10047=CARTESIAN_POINT('',(-49.,25.,50.));
#10048=CARTESIAN_POINT('',(-50.,45.,49.));
#10049=CARTESIAN_POINT('Origin',(-49.,44.5857864376269,49.));
#10050=CARTESIAN_POINT('',(-50.,25.,49.));
#10051=CARTESIAN_POINT('Origin',(-46.7928932188135,46.7928932188135,49.));
#10052=CARTESIAN_POINT('',(-45.,50.,49.));
#10053=CARTESIAN_POINT('',(-47.5,47.5,49.));
#10054=CARTESIAN_POINT('',(-44.5857864376269,49.,50.));
#10055=CARTESIAN_POINT('',(-46.7928932188135,46.7928932188135,50.));
#10056=CARTESIAN_POINT('Origin',(-44.5857864376269,49.,49.));
#10057=CARTESIAN_POINT('Origin',(25.,49.,49.));
#10058=CARTESIAN_POINT('',(45.,50.,49.));
#10059=CARTESIAN_POINT('',(25.,50.,49.));
#10060=CARTESIAN_POINT('',(44.5857864376269,49.,50.));
#10061=CARTESIAN_POINT('',(25.,49.,50.));
#10062=CARTESIAN_POINT('Origin',(44.5857864376269,49.,49.));
#10063=CARTESIAN_POINT('Origin',(46.7928932188135,46.7928932188135,49.));
#10064=CARTESIAN_POINT('',(50.,45.,49.));
#10065=CARTESIAN_POINT('',(47.5,47.5,49.));
#10066=CARTESIAN_POINT('',(49.,44.5857864376269,50.));
#10067=CARTESIAN_POINT('',(46.7928932188135,46.7928932188135,50.));
#10068=CARTESIAN_POINT('Origin',(49.,44.5857864376269,49.));
#10069=CARTESIAN_POINT('Origin',(49.,-15.,49.));
#10070=CARTESIAN_POINT('',(50.,-25.,49.));
#10071=CARTESIAN_POINT('',(50.,-15.,49.));
#10072=CARTESIAN_POINT('',(49.,-24.5857864376269,50.));
#10073=CARTESIAN_POINT('',(49.,-15.,50.));
#10074=CARTESIAN_POINT('Origin',(49.,-24.5857864376269,49.));
#10075=CARTESIAN_POINT('Origin',(41.7928932188135,-31.7928932188135,49.));
#10076=CARTESIAN_POINT('',(42.5,-32.5,49.));
#10077=CARTESIAN_POINT('',(44.5857864376269,-29.,50.));
#10078=CARTESIAN_POINT('',(41.7928932188135,-31.7928932188135,50.));
#10079=CARTESIAN_POINT('Origin',(44.5857864376269,-29.,49.));
#10080=CARTESIAN_POINT('Origin',(15.,-29.,49.));
#10081=CARTESIAN_POINT('',(34.5857864376269,-29.,50.));
#10082=CARTESIAN_POINT('',(15.,-29.,50.));
#10083=CARTESIAN_POINT('Origin',(34.5857864376269,-29.,49.));
#10084=CARTESIAN_POINT('Origin',(31.7928932188135,-31.7928932188135,49.));
#10085=CARTESIAN_POINT('',(31.7928932188135,-31.7928932188135,50.));
#10086=CARTESIAN_POINT('Origin',(47.5,47.5,35.));
#10087=CARTESIAN_POINT('',(45.,50.,35.));
#10088=CARTESIAN_POINT('',(50.,45.,35.));
#10089=CARTESIAN_POINT('Origin',(50.,-30.,35.));
#10090=CARTESIAN_POINT('',(50.,-25.,35.));
#10091=CARTESIAN_POINT('Origin',(47.5,-27.5,35.));
#10092=CARTESIAN_POINT('Origin',(0.,0.,50.));
#10093=CARTESIAN_POINT('Origin',(-47.5,47.5,35.));
#10094=CARTESIAN_POINT('',(-50.,45.,35.));
#10095=CARTESIAN_POINT('',(-45.,50.,35.));
#10096=CARTESIAN_POINT('Origin',(50.,50.,35.));
#10097=CARTESIAN_POINT('Origin',(-50.,50.,35.));
#10098=CARTESIAN_POINT('',(0.,0.,0.));
#10099=CARTESIAN_POINT('',(0.,0.,0.));
#10100=CARTESIAN_POINT('',(0.,0.,0.));
#10101=CARTESIAN_POINT('',(0.,0.,0.));
#10102=CARTESIAN_POINT('',(0.,0.,0.));
#10103=CARTESIAN_POINT('',(0.,0.,0.));
#10104=CARTESIAN_POINT('',(0.,0.,0.));
#10105=CARTESIAN_POINT('',(0.,0.,0.));
#10106=CARTESIAN_POINT('',(0.,0.,0.));
#10107=CARTESIAN_POINT('',(0.,0.,0.));
#10108=UNCERTAINTY_MEASURE_WITH_UNIT(LENGTH_MEASURE(0.01),#10132,
'DISTANCE_ACCURACY_VALUE',
'Maximum model space distance between geometric entities at asserted c
onnectivities');
#10109=UNCERTAINTY_MEASURE_WITH_UNIT(LENGTH_MEASURE(0.01),#10132,
'DISTANCE_ACCURACY_VALUE',
'Maximum model space distance between geometric entities at asserted c
onnectivities');
#10110=UNCERTAINTY_MEASURE_WITH_UNIT(LENGTH_MEASURE(0.01),#10132,
'DISTANCE_ACCURACY_VALUE',
'Maximum model space distance between geometric entities at asserted c
onnectivities');
#10111=UNCERTAINTY_MEASURE_WITH_UNIT(LENGTH_MEASURE(0.01),#10132,
'DISTANCE_ACCURACY_VALUE',
'Maximum model space distance between geometric entities at asserted c
onnectivities');
#10112=UNCERTAINTY_MEASURE_WITH_UNIT(LENGTH_MEASURE(0.01),#10132,
'DISTANCE_ACCURACY_VALUE',
'Maximum model space distance between geometric entities at asserted c
onnectivities');
#10113=UNCERTAINTY_MEASURE_WITH_UNIT(LENGTH_MEASURE(0.01),#10132,
'DISTANCE_ACCURACY_VALUE',
'Maximum model space distance between geometric entities at asserted c
onnectivities');
#10114=UNCERTAINTY_MEASURE_WITH_UNIT(LENGTH_MEASURE(0.01),#10132,
'DISTANCE_ACCURACY_VALUE',
'Maximum model space distance between geometric entities at asserted c
onnectivities');
#10115=UNCERTAINTY_MEASURE_WITH_UNIT(LENGTH_MEASURE(0.01),#10132,
'DISTANCE_ACCURACY_VALUE',
'Maximum model space distance between geometric entities at asserted c
onnectivities');
#10116=UNCERTAINTY_MEASURE_WITH_UNIT(LENGTH_MEASURE(0.01),#10132,
'DISTANCE_ACCURACY_VALUE',
'Maximum model space distance between geometric entities at asserted c
onnectivities');
#10117=UNCERTAINTY_MEASURE_WITH_UNIT(LENGTH_MEASURE(0.01),#10132,
'DISTANCE_ACCURACY_VALUE',
'Maximum model space distance between geometric entities at asserted c
onnectivities');
#10118=UNCERTAINTY_MEASURE_WITH_UNIT(LENGTH_MEASURE(0.01),#10132,
'DISTANCE_ACCURACY_VALUE',
'Maximum model space distance between geometric entities at asserted c
onnectivities');
#10119=UNCERTAINTY_MEASURE_WITH_UNIT(LENGTH_MEASURE(0.01),#10132,
'DISTANCE_ACCURACY_VALUE',
'Maximum model space distance between geometric entities at asserted c
onnectivities');
#10120=(
GEOMETRIC_REPRESENTATION_CONTEXT(3)
GLOBAL_UNCERTAINTY_ASSIGNED_CONTEXT((#10108))
GLOBAL_UNIT_ASSIGNED_CONTEXT((#10132,#10134,#10135))
REPRESENTATION_CONTEXT('','3D')
);
#10121=(
GEOMETRIC_REPRESENTATION_CONTEXT(3)
GLOBAL_UNCERTAINTY_ASSIGNED_CONTEXT((#10109))
GLOBAL_UNIT_ASSIGNED_CONTEXT((#10132,#10134,#10135))
REPRESENTATION_CONTEXT('','3D')
);
#10122=(
GEOMETRIC_REPRESENTATION_CONTEXT(3)
GLOBAL_UNCERTAINTY_ASSIGNED_CONTEXT((#10110))
GLOBAL_UNIT_ASSIGNED_CONTEXT((#10132,#10134,#10135))
REPRESENTATION_CONTEXT('','3D')
);
#10123=(
GEOMETRIC_REPRESENTATION_CONTEXT(3)
GLOBAL_UNCERTAINTY_ASSIGNED_CONTEXT((#10111))
GLOBAL_UNIT_ASSIGNED_CONTEXT((#10132,#10134,#10135))
REPRESENTATION_CONTEXT('','3D')
);
#10124=(
GEOMETRIC_REPRESENTATION_CONTEXT(3)
GLOBAL_UNCERTAINTY_ASSIGNED_CONTEXT((#10112))
GLOBAL_UNIT_ASSIGNED_CONTEXT((#10132,#10134,#10135))
REPRESENTATION_CONTEXT('','3D')
);
#10125=(
GEOMETRIC_REPRESENTATION_CONTEXT(3)
GLOBAL_UNCERTAINTY_ASSIGNED_CONTEXT((#10113))
GLOBAL_UNIT_ASSIGNED_CONTEXT((#10132,#10134,#10135))
REPRESENTATION_CONTEXT('','3D')
);
#10126=(
GEOMETRIC_REPRESENTATION_CONTEXT(3)
GLOBAL_UNCERTAINTY_ASSIGNED_CONTEXT((#10114))
GLOBAL_UNIT_ASSIGNED_CONTEXT((#10132,#10134,#10135))
REPRESENTATION_CONTEXT('','3D')
);
#10127=(
GEOMETRIC_REPRESENTATION_CONTEXT(3)
GLOBAL_UNCERTAINTY_ASSIGNED_CONTEXT((#10115))
GLOBAL_UNIT_ASSIGNED_CONTEXT((#10132,#10134,#10135))
REPRESENTATION_CONTEXT('','3D')
);
#10128=(
GEOMETRIC_REPRESENTATION_CONTEXT(3)
GLOBAL_UNCERTAINTY_ASSIGNED_CONTEXT((#10116))
GLOBAL_UNIT_ASSIGNED_CONTEXT((#10132,#10134,#10135))
REPRESENTATION_CONTEXT('','3D')
);
#10129=(
GEOMETRIC_REPRESENTATION_CONTEXT(3)
GLOBAL_UNCERTAINTY_ASSIGNED_CONTEXT((#10117))
GLOBAL_UNIT_ASSIGNED_CONTEXT((#10132,#10134,#10135))
REPRESENTATION_CONTEXT('','3D')
);
#10130=(
GEOMETRIC_REPRESENTATION_CONTEXT(3)
GLOBAL_UNCERTAINTY_ASSIGNED_CONTEXT((#10118))
GLOBAL_UNIT_ASSIGNED_CONTEXT((#10132,#10134,#10135))
REPRESENTATION_CONTEXT('','3D')
);
#10131=(
GEOMETRIC_REPRESENTATION_CONTEXT(3)
GLOBAL_UNCERTAINTY_ASSIGNED_CONTEXT((#10119))
GLOBAL_UNIT_ASSIGNED_CONTEXT((#10132,#10134,#10135))
REPRESENTATION_CONTEXT('','3D')
);
#10132=(
LENGTH_UNIT()
NAMED_UNIT(*)
SI_UNIT(.MILLI.,.METRE.)
);
#10133=(
LENGTH_UNIT()
NAMED_UNIT(*)
SI_UNIT($,.METRE.)
);
#10134=(
NAMED_UNIT(*)
PLANE_ANGLE_UNIT()
SI_UNIT($,.RADIAN.)
);
#10135=(
NAMED_UNIT(*)
SI_UNIT($,.STERADIAN.)
SOLID_ANGLE_UNIT()
);
#10136=SHAPE_DEFINITION_REPRESENTATION(#10147,#10168);
#10137=SHAPE_DEFINITION_REPRESENTATION(#10148,#10169);
#10138=SHAPE_DEFINITION_REPRESENTATION(#10149,#10170);
#10139=SHAPE_DEFINITION_REPRESENTATION(#10150,#10171);
#10140=SHAPE_DEFINITION_REPRESENTATION(#10151,#10172);
#10141=SHAPE_DEFINITION_REPRESENTATION(#10152,#10173);
#10142=SHAPE_DEFINITION_REPRESENTATION(#10153,#10174);
#10143=SHAPE_DEFINITION_REPRESENTATION(#10154,#10175);
#10144=SHAPE_DEFINITION_REPRESENTATION(#10155,#10176);
#10145=SHAPE_DEFINITION_REPRESENTATION(#10156,#10177);
#10146=SHAPE_DEFINITION_REPRESENTATION(#10157,#10178);
#10147=PRODUCT_DEFINITION_SHAPE('',$,#10180);
#10148=PRODUCT_DEFINITION_SHAPE('',$,#10181);
#10149=PRODUCT_DEFINITION_SHAPE('',$,#10182);
#10150=PRODUCT_DEFINITION_SHAPE('',$,#10183);
#10151=PRODUCT_DEFINITION_SHAPE('',$,#10184);
#10152=PRODUCT_DEFINITION_SHAPE('',$,#10185);
#10153=PRODUCT_DEFINITION_SHAPE('',$,#10186);
#10154=PRODUCT_DEFINITION_SHAPE('',$,#10187);
#10155=PRODUCT_DEFINITION_SHAPE('',$,#10188);
#10156=PRODUCT_DEFINITION_SHAPE('',$,#10189);
#10157=PRODUCT_DEFINITION_SHAPE('',$,#10190);
#10158=PRODUCT_DEFINITION_SHAPE($,$,#41);
#10159=PRODUCT_DEFINITION_SHAPE($,$,#42);
#10160=PRODUCT_DEFINITION_SHAPE($,$,#43);
#10161=PRODUCT_DEFINITION_SHAPE($,$,#44);
#10162=PRODUCT_DEFINITION_SHAPE($,$,#45);
#10163=PRODUCT_DEFINITION_SHAPE($,$,#46);
#10164=PRODUCT_DEFINITION_SHAPE($,$,#47);
#10165=PRODUCT_DEFINITION_SHAPE($,$,#48);
#10166=PRODUCT_DEFINITION_SHAPE($,$,#49);
#10167=PRODUCT_DEFINITION_SHAPE($,$,#50);
#10168=SHAPE_REPRESENTATION('',(#6000,#6612,#6613,#6614,#6615,#6616,#6617,
#6618,#6619,#6620,#6621),#10120);
#10169=SHAPE_REPRESENTATION('',(#6001),#10121);
#10170=SHAPE_REPRESENTATION('',(#6044),#10122);
#10171=SHAPE_REPRESENTATION('',(#6074),#10123);
#10172=SHAPE_REPRESENTATION('',(#6173),#10124);
#10173=SHAPE_REPRESENTATION('',(#6236),#10125);
#10174=SHAPE_REPRESENTATION('',(#6309),#10126);
#10175=SHAPE_REPRESENTATION('',(#6326),#10127);
#10176=SHAPE_REPRESENTATION('',(#6399),#10128);
#10177=SHAPE_REPRESENTATION('',(#6474),#10129);
#10178=SHAPE_REPRESENTATION('',(#6549),#10130);
#10179=PRODUCT_DEFINITION_CONTEXT('part definition',#10214,'design');
#10180=PRODUCT_DEFINITION('MAS-266','MAS-266',#10191,#10179);
#10181=PRODUCT_DEFINITION('Base','Base',#10192,#10179);
#10182=PRODUCT_DEFINITION('Side_Block','Side_Block',#10193,#10179);
#10183=PRODUCT_DEFINITION('Top_Block','Top_Block',#10194,#10179);
#10184=PRODUCT_DEFINITION('Bottom_Block_01','Bottom_Block_01',#10195,#10179);
#10185=PRODUCT_DEFINITION('Front_Block_02','Front_Block_02',#10196,#10179);
#10186=PRODUCT_DEFINITION('Front_Mount','Front_Mount',#10197,#10179);
#10187=PRODUCT_DEFINITION('Front_Block_01','Front_Block_01',#10198,#10179);
#10188=PRODUCT_DEFINITION('Middle_Block_01','Middle_Block_01',#10199,#10179);
#10189=PRODUCT_DEFINITION('Middle_Block_02','Middle_Block_02',#10200,#10179);
#10190=PRODUCT_DEFINITION('Bottom_Block_02','Bottom_Block_02',#10201,#10179);
#10191=PRODUCT_DEFINITION_FORMATION('',$,#10216);
#10192=PRODUCT_DEFINITION_FORMATION('',$,#10217);
#10193=PRODUCT_DEFINITION_FORMATION('',$,#10218);
#10194=PRODUCT_DEFINITION_FORMATION('',$,#10219);
#10195=PRODUCT_DEFINITION_FORMATION('',$,#10220);
#10196=PRODUCT_DEFINITION_FORMATION('',$,#10221);
#10197=PRODUCT_DEFINITION_FORMATION('',$,#10222);
#10198=PRODUCT_DEFINITION_FORMATION('',$,#10223);
#10199=PRODUCT_DEFINITION_FORMATION('',$,#10224);
#10200=PRODUCT_DEFINITION_FORMATION('',$,#10225);
#10201=PRODUCT_DEFINITION_FORMATION('',$,#10226);
#10202=PRODUCT_RELATED_PRODUCT_CATEGORY('MAS-266','MAS-266',(#10216));
#10203=PRODUCT_RELATED_PRODUCT_CATEGORY('Base','Base',(#10217));
#10204=PRODUCT_RELATED_PRODUCT_CATEGORY('Side_Block','Side_Block',(#10218));
#10205=PRODUCT_RELATED_PRODUCT_CATEGORY('Top_Block','Top_Block',(#10219));
#10206=PRODUCT_RELATED_PRODUCT_CATEGORY('Bottom_Block_01',
'Bottom_Block_01',(#10220));
#10207=PRODUCT_RELATED_PRODUCT_CATEGORY('Front_Block_02',
'Front_Block_02',(#10221));
#10208=PRODUCT_RELATED_PRODUCT_CATEGORY('Front_Mount','Front_Mount',(#10222));
#10209=PRODUCT_RELATED_PRODUCT_CATEGORY('Front_Block_01',
'Front_Block_01',(#10223));
#10210=PRODUCT_RELATED_PRODUCT_CATEGORY('Middle_Block_01',
'Middle_Block_01',(#10224));
#10211=PRODUCT_RELATED_PRODUCT_CATEGORY('Middle_Block_02',
'Middle_Block_02',(#10225));
#10212=PRODUCT_RELATED_PRODUCT_CATEGORY('Bottom_Block_02',
'Bottom_Block_02',(#10226));
#10213=APPLICATION_PROTOCOL_DEFINITION('international standard',
'automotive_design',2009,#10214);
#10214=APPLICATION_CONTEXT(
'Core Data for Automotive Mechanical Design Process');
#10215=PRODUCT_CONTEXT('part definition',#10214,'mechanical');
#10216=PRODUCT('MAS-266','MAS-266',$,(#10215));
#10217=PRODUCT('Base','Base',$,(#10215));
#10218=PRODUCT('Side_Block','Side_Block',$,(#10215));
#10219=PRODUCT('Top_Block','Top_Block',$,(#10215));
#10220=PRODUCT('Bottom_Block_01','Bottom_Block_01',$,(#10215));
#10221=PRODUCT('Front_Block_02','Front_Block_02',$,(#10215));
#10222=PRODUCT('Front_Mount','Front_Mount',$,(#10215));
#10223=PRODUCT('Front_Block_01','Front_Block_01',$,(#10215));
#10224=PRODUCT('Middle_Block_01','Middle_Block_01',$,(#10215));
#10225=PRODUCT('Middle_Block_02','Middle_Block_02',$,(#10215));
#10226=PRODUCT('Bottom_Block_02','Bottom_Block_02',$,(#10215));
#10227=PRESENTATION_STYLE_ASSIGNMENT((#10229));
#10228=PRESENTATION_STYLE_ASSIGNMENT((#10230));
#10229=SURFACE_STYLE_USAGE(.BOTH.,#10231);
#10230=SURFACE_STYLE_USAGE(.BOTH.,#10232);
#10231=SURFACE_SIDE_STYLE('',(#10233));
#10232=SURFACE_SIDE_STYLE('',(#10234));
#10233=SURFACE_STYLE_FILL_AREA(#10235);
#10234=SURFACE_STYLE_FILL_AREA(#10236);
#10235=FILL_AREA_STYLE('Steel - Satin',(#10237));
#10236=FILL_AREA_STYLE('Steel - Satin',(#10238));
#10237=FILL_AREA_STYLE_COLOUR('Steel - Satin',#10239);
#10238=FILL_AREA_STYLE_COLOUR('Steel - Satin',#10240);
#10239=COLOUR_RGB('Steel - Satin',0.627450980392157,0.627450980392157,0.627450980392157);
#10240=COLOUR_RGB('Steel - Satin',0.329411764705882,0.329411764705882,0.329411764705882);
#10241=COLOUR_RGB('Dark Blue',0.08,0.2,0.34);
#10242=FILL_AREA_STYLE_COLOUR('',#10241);
#10243=FILL_AREA_STYLE('',(#10242));
#10244=SURFACE_STYLE_FILL_AREA(#10243);
#10245=SURFACE_SIDE_STYLE('',(#10244));
#10246=SURFACE_STYLE_USAGE(.BOTH.,#10245);
#10247=PRESENTATION_STYLE_ASSIGNMENT((#10246));
#10248=COLOUR_RGB('Light Blue',0.38,0.62,0.78);
#10249=FILL_AREA_STYLE_COLOUR('',#10248);
#10250=FILL_AREA_STYLE('',(#10249));
#10251=SURFACE_STYLE_FILL_AREA(#10250);
#10252=SURFACE_SIDE_STYLE('',(#10251));
#10253=SURFACE_STYLE_USAGE(.BOTH.,#10252);
#10254=PRESENTATION_STYLE_ASSIGNMENT((#10253));
#10255=COLOUR_RGB('Sky Blue',0.24,0.69,0.87);
#10256=FILL_AREA_STYLE_COLOUR('',#10255);
#10257=FILL_AREA_STYLE('',(#10256));
#10258=SURFACE_STYLE_FILL_AREA(#10257);
#10259=SURFACE_SIDE_STYLE('',(#10258));
#10260=SURFACE_STYLE_USAGE(.BOTH.,#10259);
#10261=PRESENTATION_STYLE_ASSIGNMENT((#10260));
#10262=COLOUR_RGB('Grey',0.48,0.52,0.57);
#10263=FILL_AREA_STYLE_COLOUR('',#10262);
#10264=FILL_AREA_STYLE('',(#10263));
#10265=SURFACE_STYLE_FILL_AREA(#10264);
#10266=SURFACE_SIDE_STYLE('',(#10265));
#10267=SURFACE_STYLE_USAGE(.BOTH.,#10266);
#10268=PRESENTATION_STYLE_ASSIGNMENT((#10267));
#10269=COLOUR_RGB('Black',0.12,0.14,0.17);
#10270=FILL_AREA_STYLE_COLOUR('',#10269);
#10271=FILL_AREA_STYLE('',(#10270));
#10272=SURFACE_STYLE_FILL_AREA(#10271);
#10273=SURFACE_SIDE_STYLE('',(#10272));
#10274=SURFACE_STYLE_USAGE(.BOTH.,#10273);
#10275=PRESENTATION_STYLE_ASSIGNMENT((#10274));
#10276=COLOUR_RGB('Off White',0.89,0.88,0.83);
#10277=FILL_AREA_STYLE_COLOUR('',#10276);
#10278=FILL_AREA_STYLE('',(#10277));
#10279=SURFACE_STYLE_FILL_AREA(#10278);
#10280=SURFACE_SIDE_STYLE('',(#10279));
#10281=SURFACE_STYLE_USAGE(.BOTH.,#10280);
#10282=PRESENTATION_STYLE_ASSIGNMENT((#10281));
ENDSEC;
END-ISO-10303-21;
